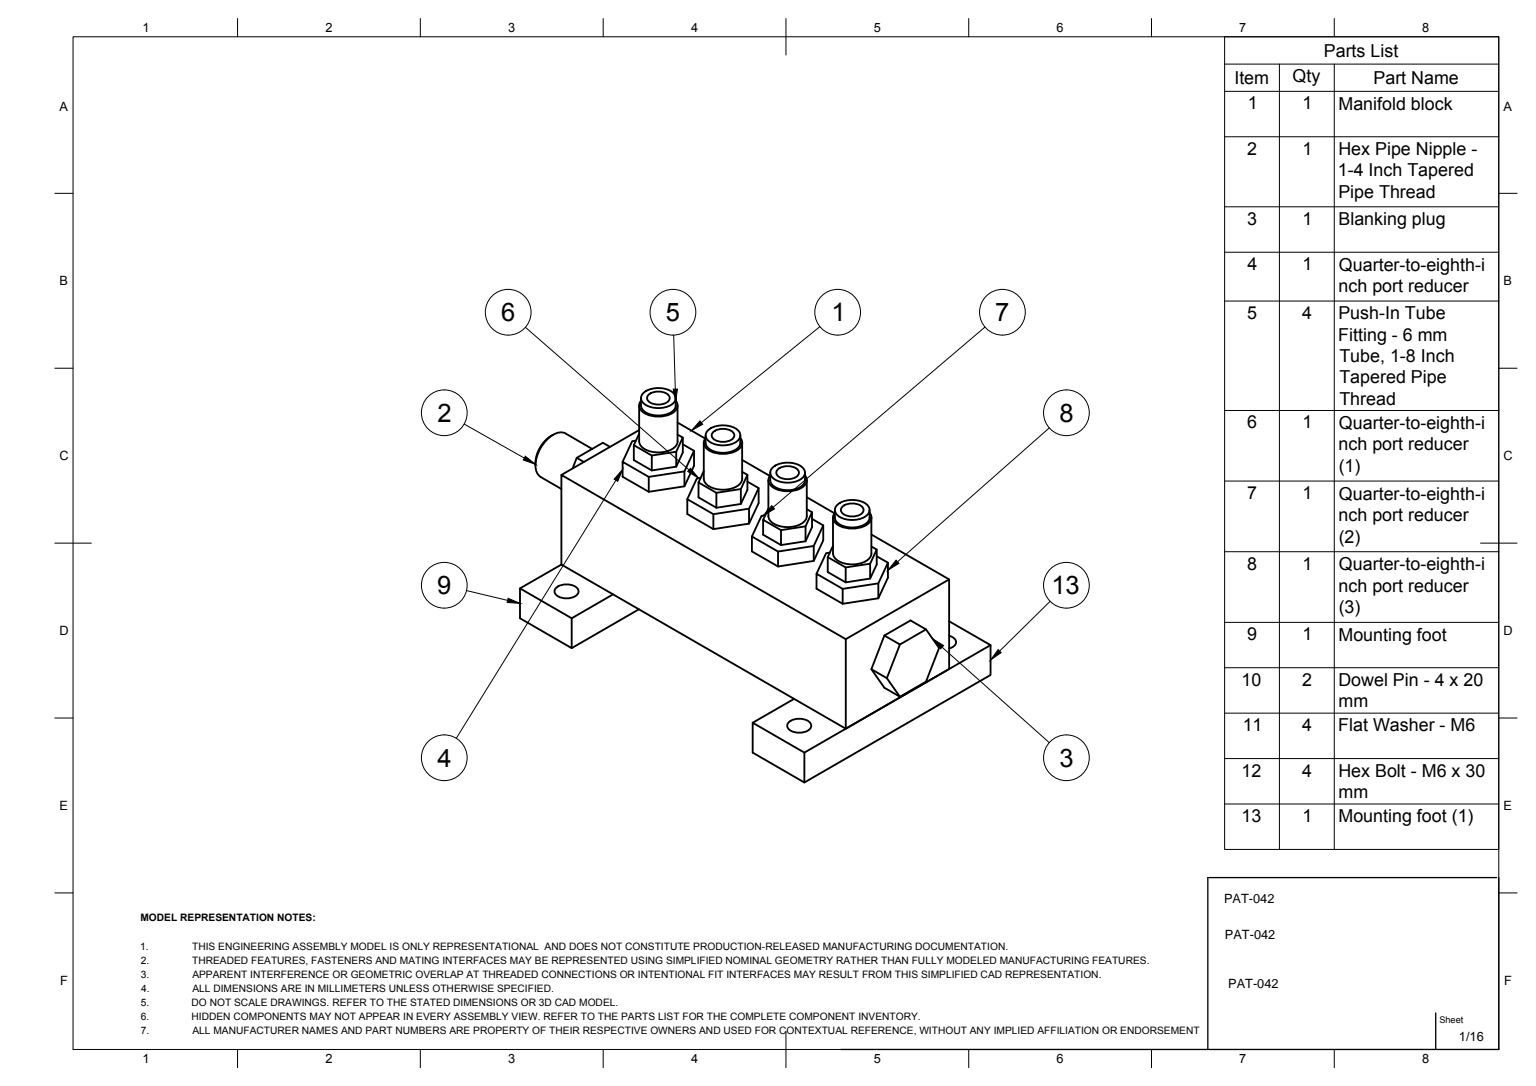
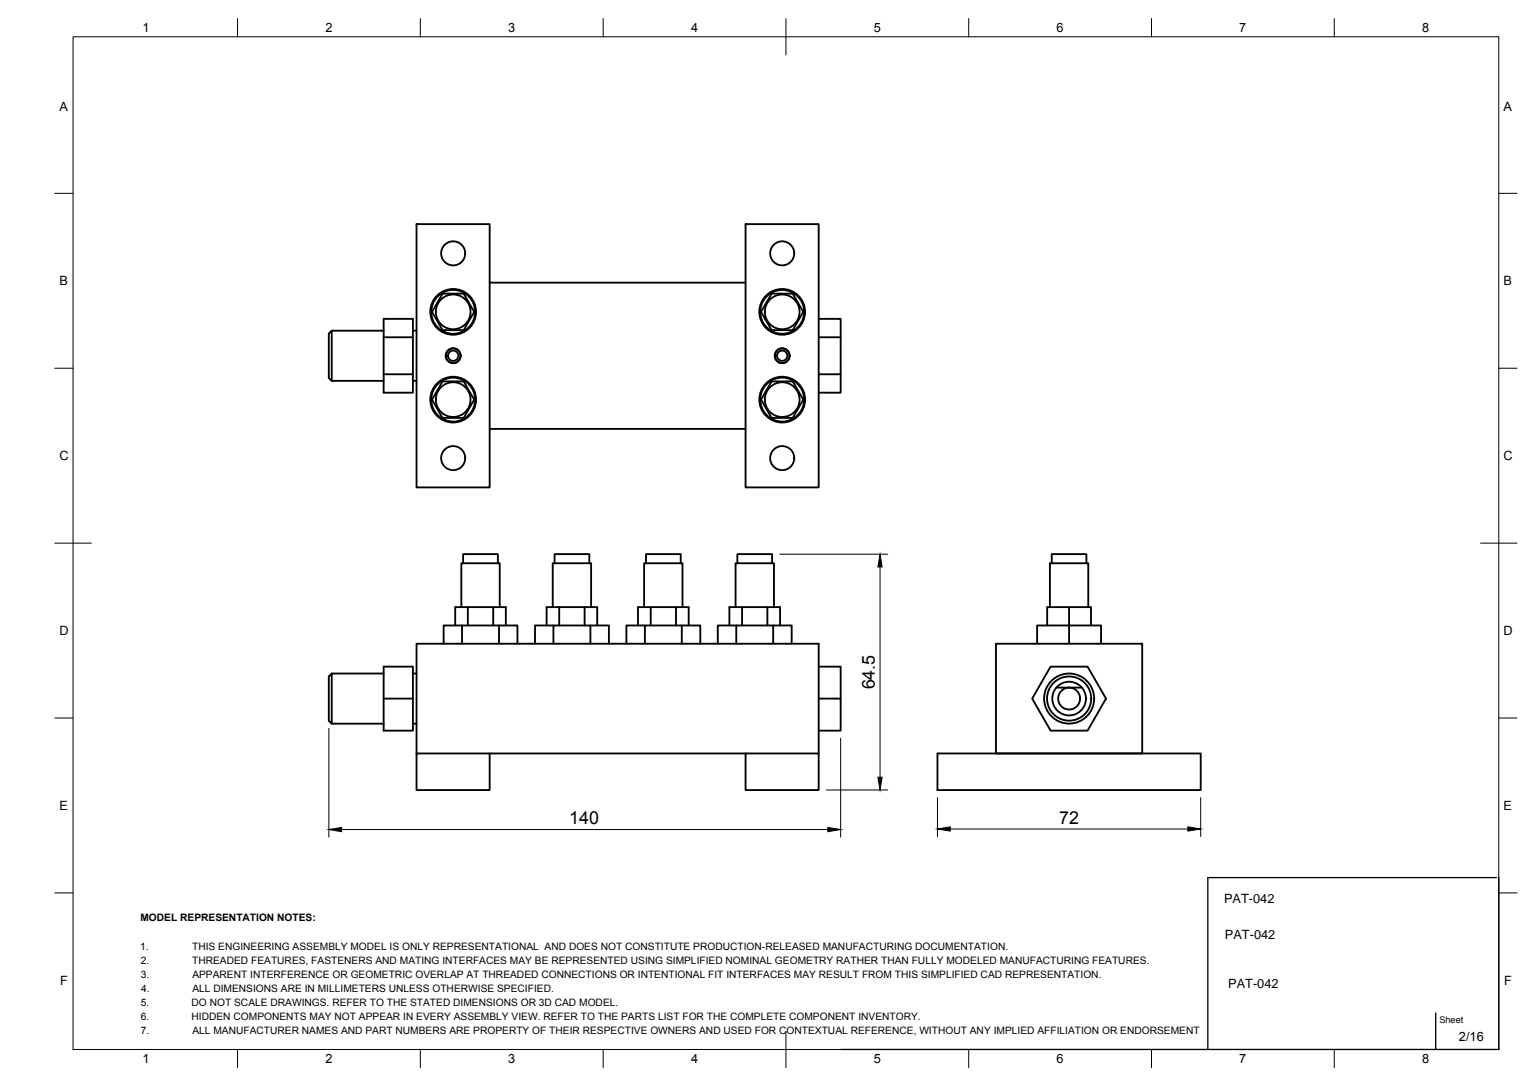
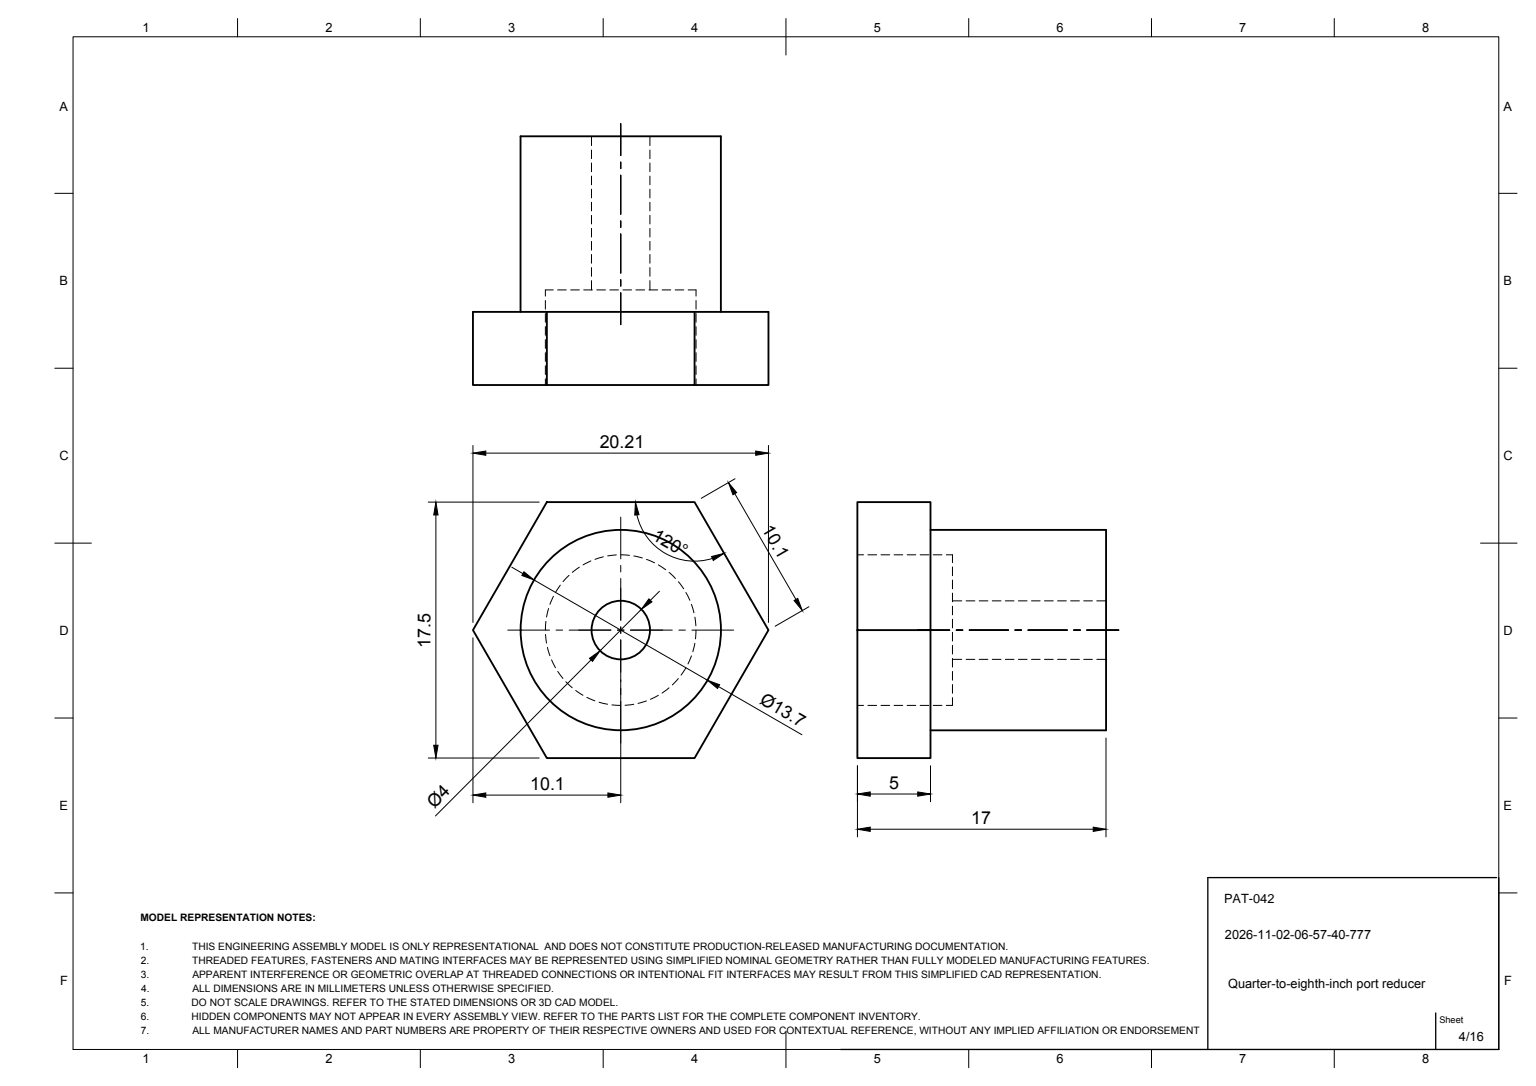
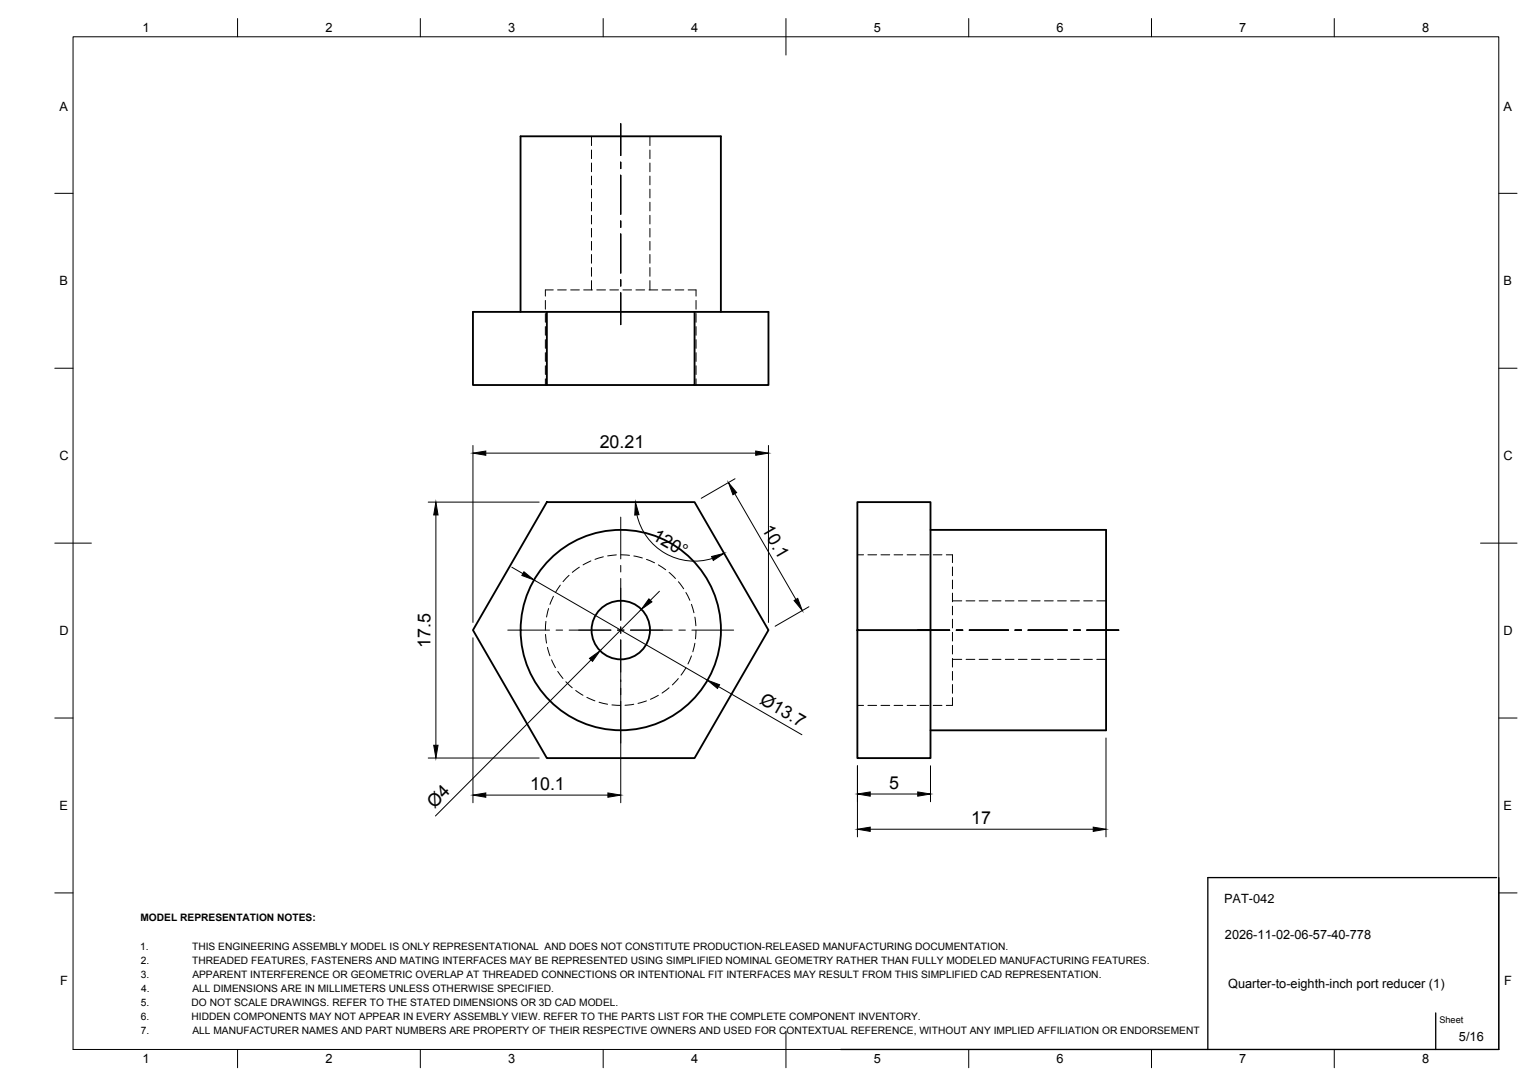
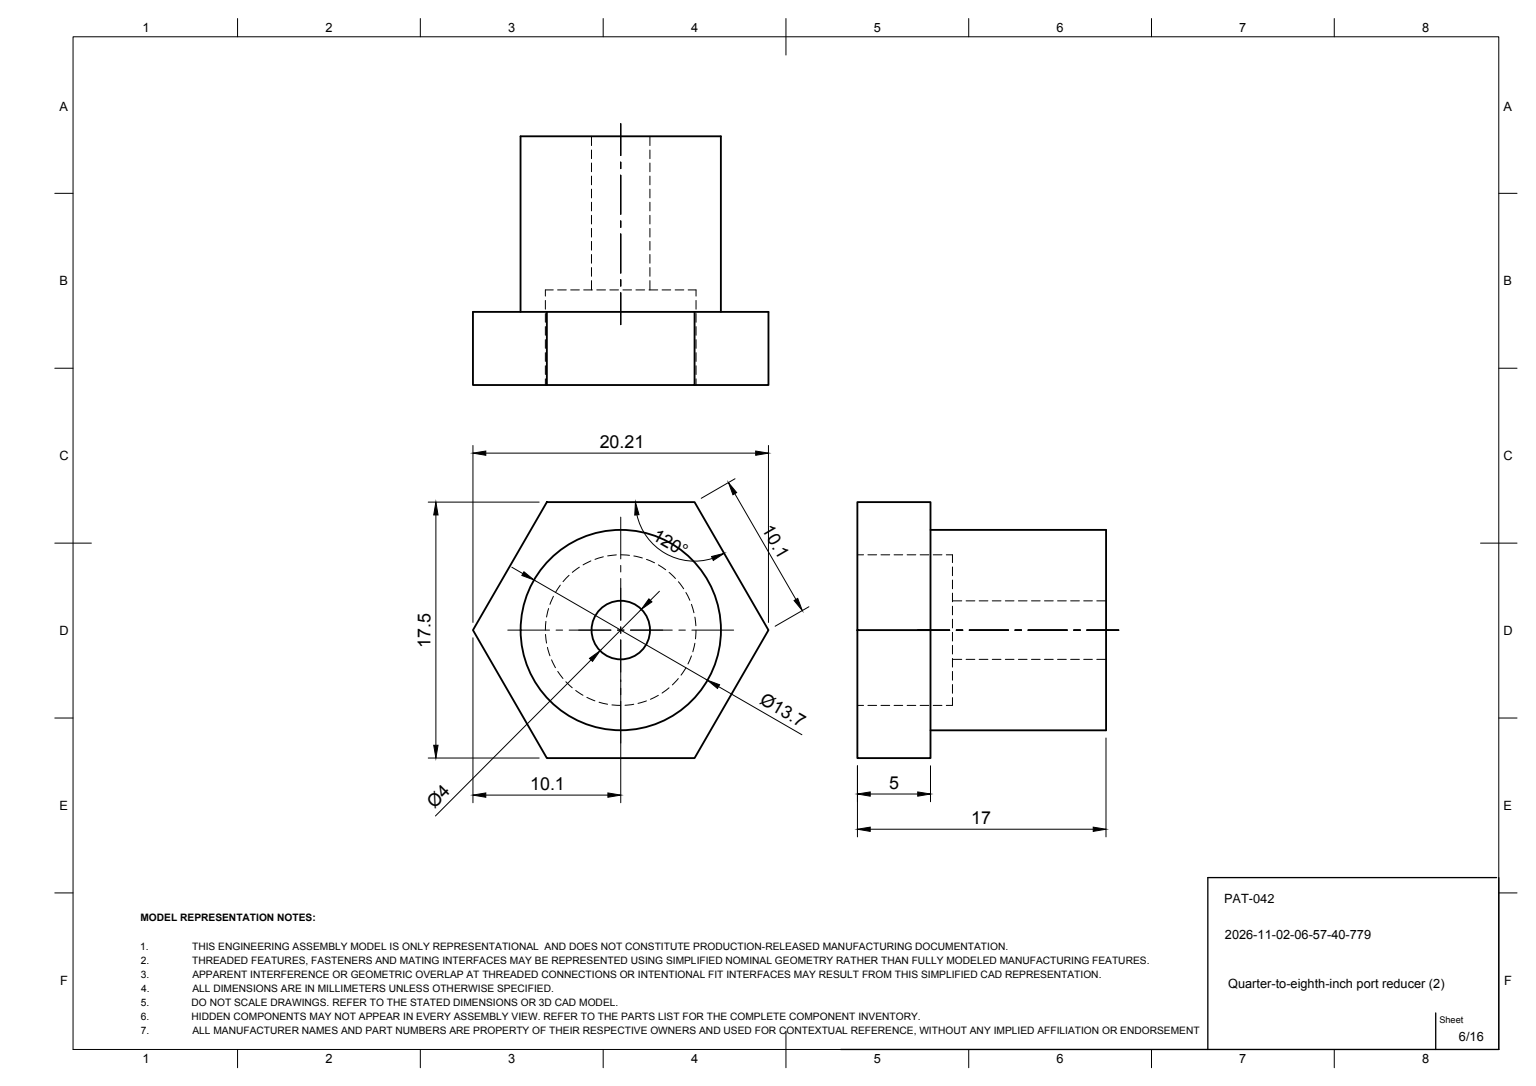
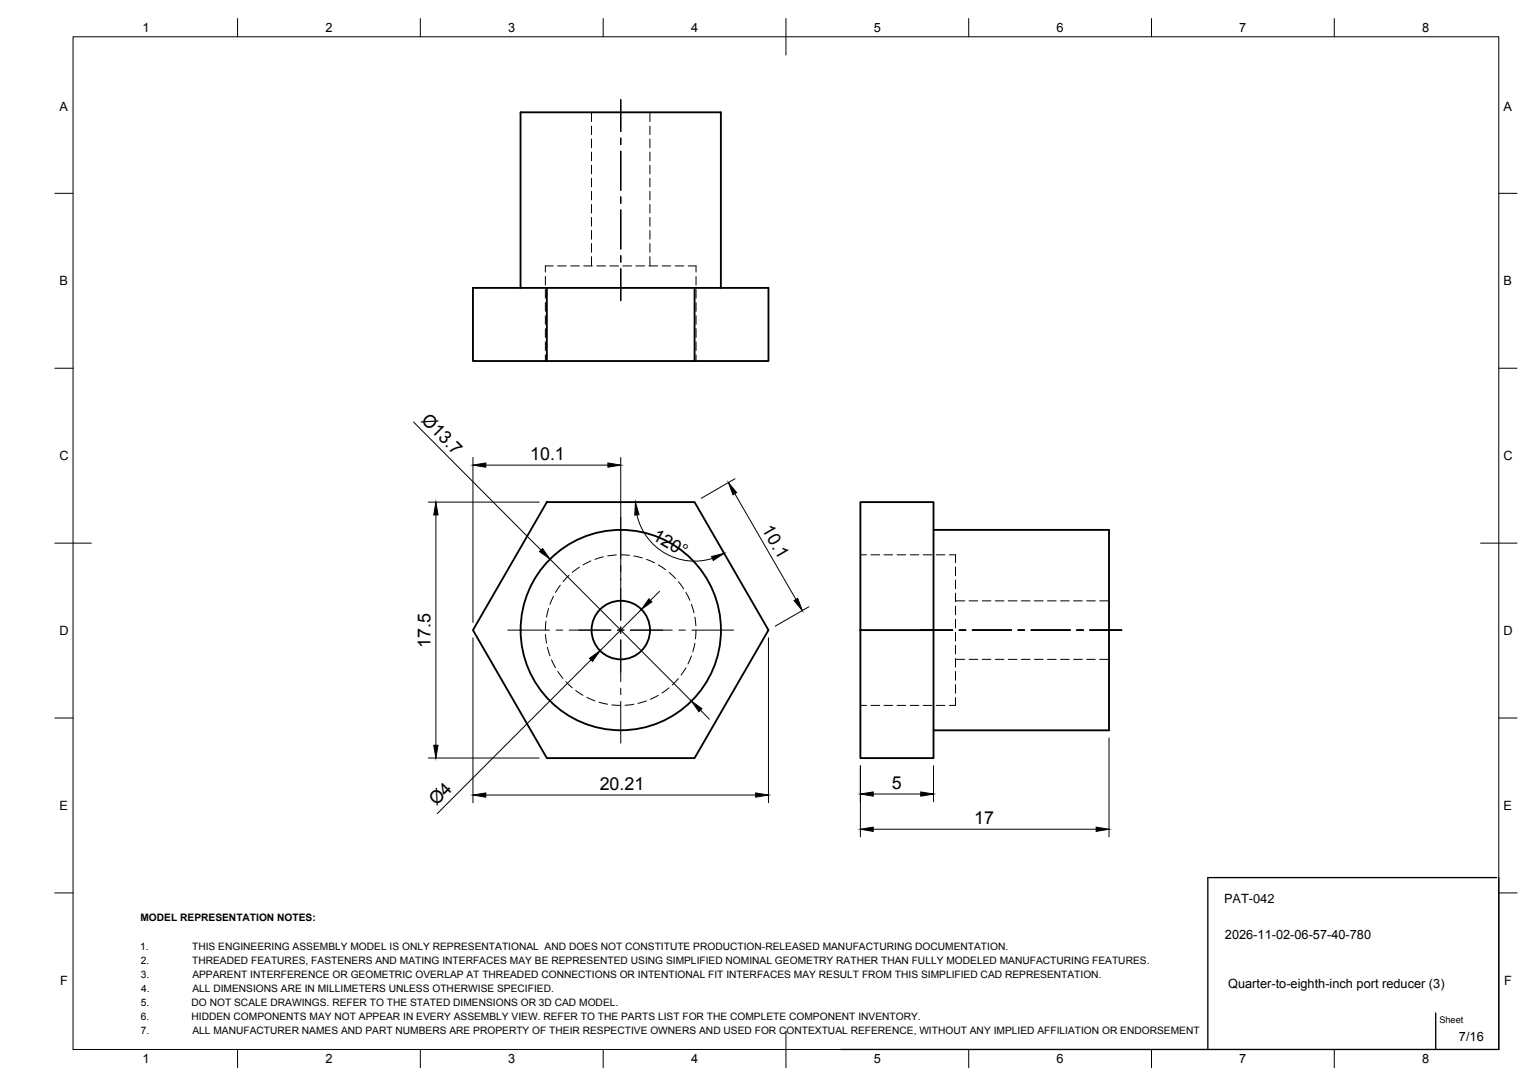
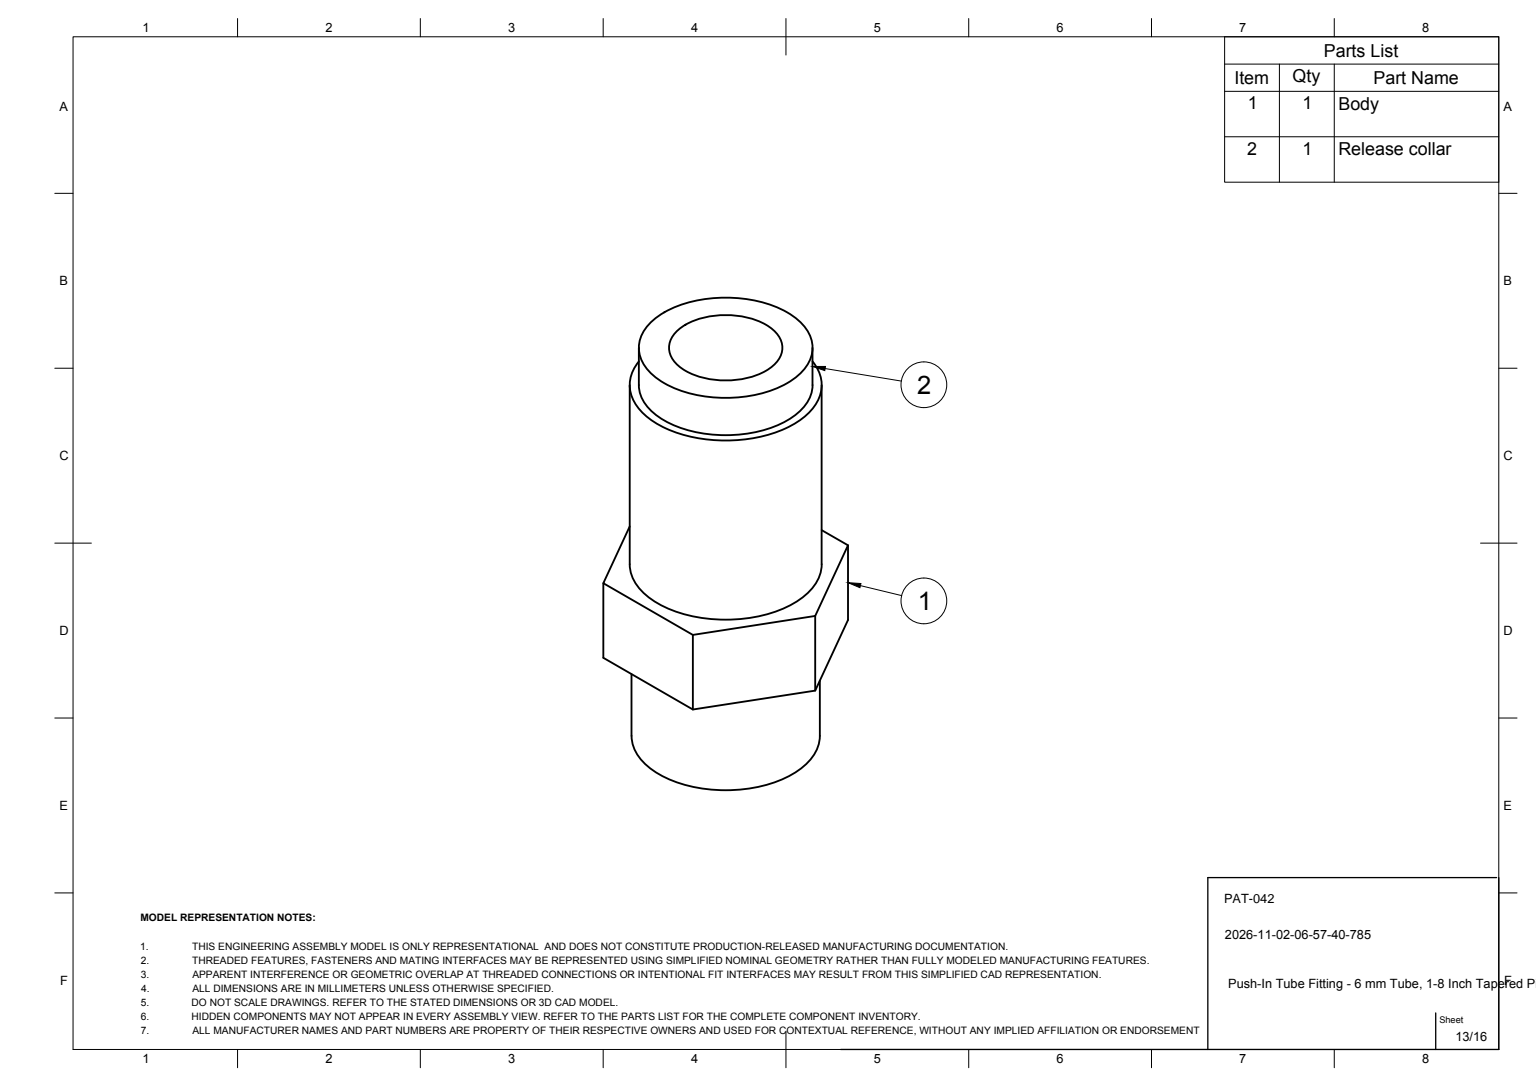
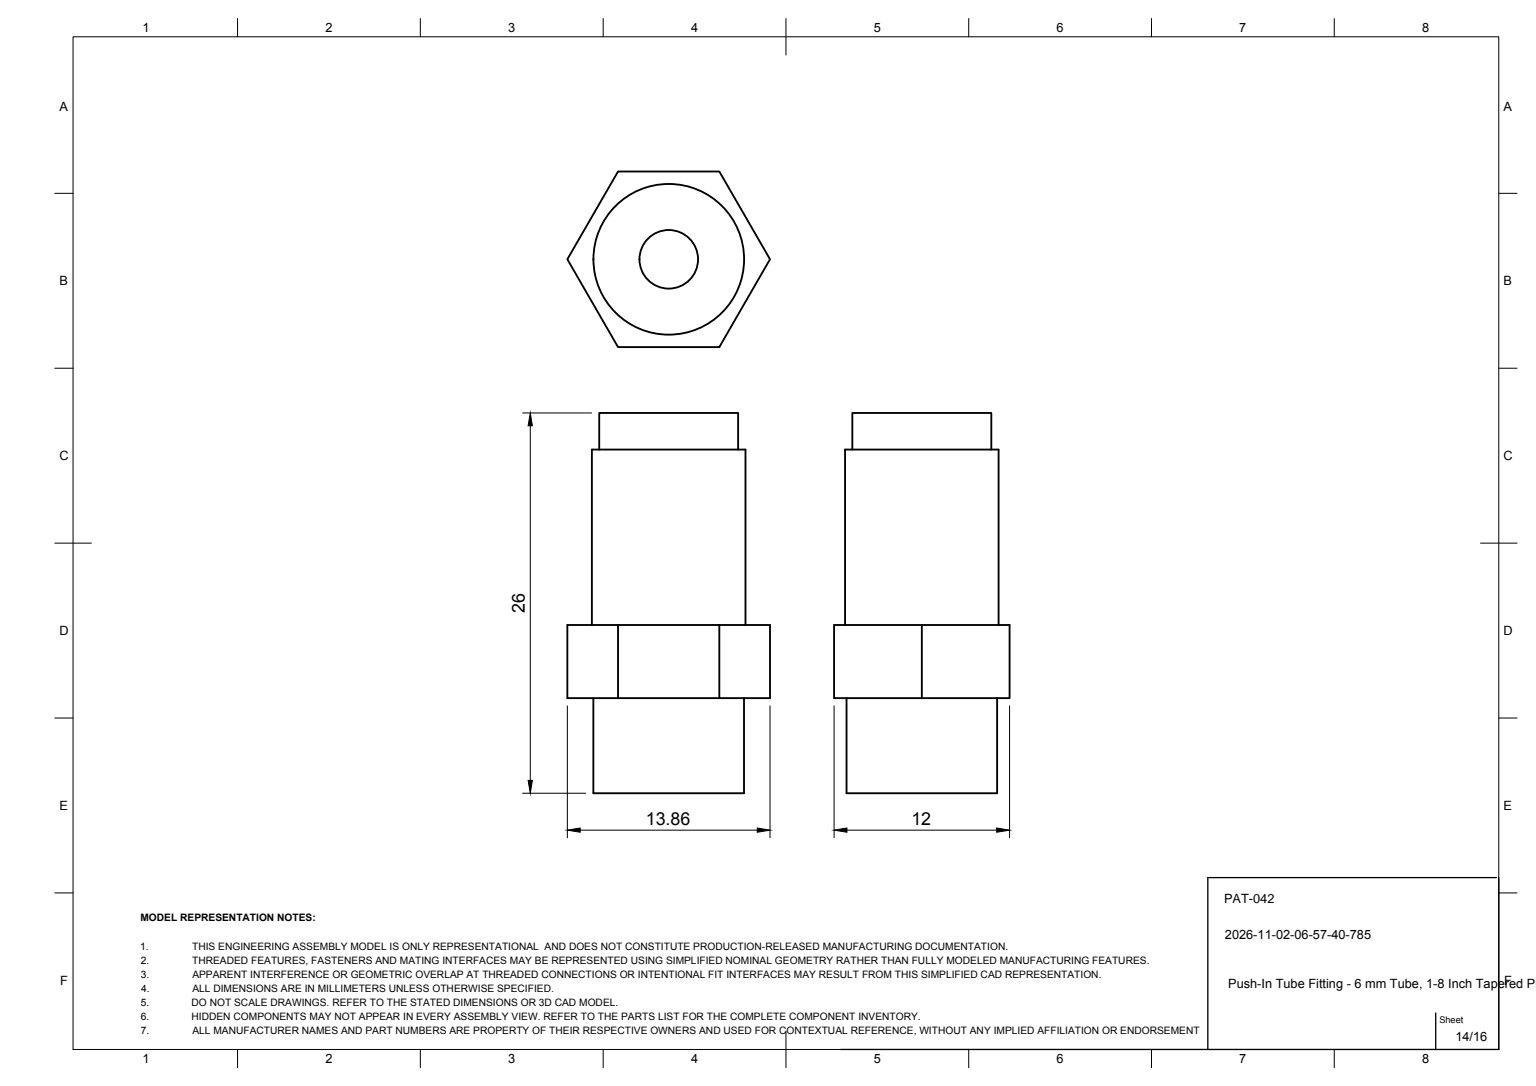
ISO-10303-21;
HEADER;
/* Generated by software containing ST-Developer
 * from STEP Tools, Inc. (www.steptools.com) 
 */

FILE_DESCRIPTION(
/* description */ ('Manifold and mounting hardware'),
/* implementation_level */ '2;1');

FILE_NAME(
/* name */ 'PAT-042',
/* time_stamp */ '2026-10-28T21:46:49-07:00',
/* author */ (''),
/* organization */ (''),
/* preprocessor_version */ 'ST-DEVELOPER v20.2',
/* originating_system */ 'Autodesk Translation Framework v15.17.0.0',
/* authorisation */ '');

FILE_SCHEMA (('AUTOMOTIVE_DESIGN { 1 0 10303 214 3 1 1 }'));
ENDSEC;

DATA;
#10=MECHANICAL_DESIGN_GEOMETRIC_PRESENTATION_REPRESENTATION('',(#150,#151,
#152,#153,#154,#155,#156,#157,#158,#159,#160,#161,#162,#163),#5638);
#11=(
BOUNDED_CURVE()
B_SPLINE_CURVE(2,(#5534,#5535,#5536),.UNSPECIFIED.,.F.,.F.)
B_SPLINE_CURVE_WITH_KNOTS((3,3),(0.144988513094728,0.791574906712449),
 .UNSPECIFIED.)
CURVE()
GEOMETRIC_REPRESENTATION_ITEM()
RATIONAL_B_SPLINE_CURVE((1.09282032302755,1.26188021535082,1.09282032302931))
REPRESENTATION_ITEM('')
);
#12=(
BOUNDED_CURVE()
B_SPLINE_CURVE(2,(#5538,#5539,#5540),.UNSPECIFIED.,.F.,.F.)
B_SPLINE_CURVE_WITH_KNOTS((3,3),(0.144988513094728,0.791574906712449),
 .UNSPECIFIED.)
CURVE()
GEOMETRIC_REPRESENTATION_ITEM()
RATIONAL_B_SPLINE_CURVE((1.09282032302755,1.26188021535082,1.09282032302931))
REPRESENTATION_ITEM('')
);
#13=(
BOUNDED_CURVE()
B_SPLINE_CURVE(2,(#5542,#5543,#5544),.UNSPECIFIED.,.F.,.F.)
B_SPLINE_CURVE_WITH_KNOTS((3,3),(0.144988513094728,0.791574906712449),
 .UNSPECIFIED.)
CURVE()
GEOMETRIC_REPRESENTATION_ITEM()
RATIONAL_B_SPLINE_CURVE((1.09282032302755,1.26188021535082,1.09282032302931))
REPRESENTATION_ITEM('')
);
#14=(
BOUNDED_CURVE()
B_SPLINE_CURVE(2,(#5546,#5547,#5548),.UNSPECIFIED.,.F.,.F.)
B_SPLINE_CURVE_WITH_KNOTS((3,3),(0.144988513094728,0.791574906712449),
 .UNSPECIFIED.)
CURVE()
GEOMETRIC_REPRESENTATION_ITEM()
RATIONAL_B_SPLINE_CURVE((1.09282032302755,1.26188021535082,1.09282032302931))
REPRESENTATION_ITEM('')
);
#15=(
BOUNDED_CURVE()
B_SPLINE_CURVE(2,(#5550,#5551,#5552),.UNSPECIFIED.,.F.,.F.)
B_SPLINE_CURVE_WITH_KNOTS((3,3),(0.144988513094728,0.791574906712449),
 .UNSPECIFIED.)
CURVE()
GEOMETRIC_REPRESENTATION_ITEM()
RATIONAL_B_SPLINE_CURVE((1.09282032302755,1.26188021535082,1.09282032302931))
REPRESENTATION_ITEM('')
);
#16=(
BOUNDED_CURVE()
B_SPLINE_CURVE(2,(#5553,#5554,#5555),.UNSPECIFIED.,.F.,.F.)
B_SPLINE_CURVE_WITH_KNOTS((3,3),(0.144988513094727,0.791574906712449),
 .UNSPECIFIED.)
CURVE()
GEOMETRIC_REPRESENTATION_ITEM()
RATIONAL_B_SPLINE_CURVE((1.09282032302755,1.26188021535082,1.09282032302931))
REPRESENTATION_ITEM('')
);
#17=SPHERICAL_SURFACE('',#3616,0.399999999999996);
#18=ITEM_DEFINED_TRANSFORMATION($,$,#3572,#3613);
#19=ITEM_DEFINED_TRANSFORMATION($,$,#3600,#3614);
#20=ITEM_DEFINED_TRANSFORMATION($,$,#3310,#3649);
#21=ITEM_DEFINED_TRANSFORMATION($,$,#3396,#3650);
#22=ITEM_DEFINED_TRANSFORMATION($,$,#3416,#3651);
#23=ITEM_DEFINED_TRANSFORMATION($,$,#3436,#3652);
#24=ITEM_DEFINED_TRANSFORMATION($,$,#3456,#3653);
#25=ITEM_DEFINED_TRANSFORMATION($,$,#3476,#3654);
#26=ITEM_DEFINED_TRANSFORMATION($,$,#3506,#3655);
#27=ITEM_DEFINED_TRANSFORMATION($,$,#3536,#3656);
#28=ITEM_DEFINED_TRANSFORMATION($,$,#3558,#3657);
#29=ITEM_DEFINED_TRANSFORMATION($,$,#3571,#3658);
#30=ITEM_DEFINED_TRANSFORMATION($,$,#3571,#3659);
#31=ITEM_DEFINED_TRANSFORMATION($,$,#3571,#3660);
#32=ITEM_DEFINED_TRANSFORMATION($,$,#3571,#3661);
#33=ITEM_DEFINED_TRANSFORMATION($,$,#3615,#3662);
#34=ITEM_DEFINED_TRANSFORMATION($,$,#3623,#3663);
#35=ITEM_DEFINED_TRANSFORMATION($,$,#3632,#3664);
#36=ITEM_DEFINED_TRANSFORMATION($,$,#3623,#3665);
#37=ITEM_DEFINED_TRANSFORMATION($,$,#3632,#3666);
#38=ITEM_DEFINED_TRANSFORMATION($,$,#3615,#3667);
#39=ITEM_DEFINED_TRANSFORMATION($,$,#3623,#3668);
#40=ITEM_DEFINED_TRANSFORMATION($,$,#3632,#3669);
#41=ITEM_DEFINED_TRANSFORMATION($,$,#3623,#3670);
#42=ITEM_DEFINED_TRANSFORMATION($,$,#3632,#3671);
#43=(
REPRESENTATION_RELATIONSHIP($,$,#5711,#5710)
REPRESENTATION_RELATIONSHIP_WITH_TRANSFORMATION(#18)
SHAPE_REPRESENTATION_RELATIONSHIP()
);
#44=(
REPRESENTATION_RELATIONSHIP($,$,#5712,#5710)
REPRESENTATION_RELATIONSHIP_WITH_TRANSFORMATION(#19)
SHAPE_REPRESENTATION_RELATIONSHIP()
);
#45=(
REPRESENTATION_RELATIONSHIP($,$,#5701,#5700)
REPRESENTATION_RELATIONSHIP_WITH_TRANSFORMATION(#20)
SHAPE_REPRESENTATION_RELATIONSHIP()
);
#46=(
REPRESENTATION_RELATIONSHIP($,$,#5702,#5700)
REPRESENTATION_RELATIONSHIP_WITH_TRANSFORMATION(#21)
SHAPE_REPRESENTATION_RELATIONSHIP()
);
#47=(
REPRESENTATION_RELATIONSHIP($,$,#5703,#5700)
REPRESENTATION_RELATIONSHIP_WITH_TRANSFORMATION(#22)
SHAPE_REPRESENTATION_RELATIONSHIP()
);
#48=(
REPRESENTATION_RELATIONSHIP($,$,#5704,#5700)
REPRESENTATION_RELATIONSHIP_WITH_TRANSFORMATION(#23)
SHAPE_REPRESENTATION_RELATIONSHIP()
);
#49=(
REPRESENTATION_RELATIONSHIP($,$,#5705,#5700)
REPRESENTATION_RELATIONSHIP_WITH_TRANSFORMATION(#24)
SHAPE_REPRESENTATION_RELATIONSHIP()
);
#50=(
REPRESENTATION_RELATIONSHIP($,$,#5706,#5700)
REPRESENTATION_RELATIONSHIP_WITH_TRANSFORMATION(#25)
SHAPE_REPRESENTATION_RELATIONSHIP()
);
#51=(
REPRESENTATION_RELATIONSHIP($,$,#5707,#5700)
REPRESENTATION_RELATIONSHIP_WITH_TRANSFORMATION(#26)
SHAPE_REPRESENTATION_RELATIONSHIP()
);
#52=(
REPRESENTATION_RELATIONSHIP($,$,#5708,#5700)
REPRESENTATION_RELATIONSHIP_WITH_TRANSFORMATION(#27)
SHAPE_REPRESENTATION_RELATIONSHIP()
);
#53=(
REPRESENTATION_RELATIONSHIP($,$,#5709,#5700)
REPRESENTATION_RELATIONSHIP_WITH_TRANSFORMATION(#28)
SHAPE_REPRESENTATION_RELATIONSHIP()
);
#54=(
REPRESENTATION_RELATIONSHIP($,$,#5710,#5700)
REPRESENTATION_RELATIONSHIP_WITH_TRANSFORMATION(#29)
SHAPE_REPRESENTATION_RELATIONSHIP()
);
#55=(
REPRESENTATION_RELATIONSHIP($,$,#5710,#5700)
REPRESENTATION_RELATIONSHIP_WITH_TRANSFORMATION(#30)
SHAPE_REPRESENTATION_RELATIONSHIP()
);
#56=(
REPRESENTATION_RELATIONSHIP($,$,#5710,#5700)
REPRESENTATION_RELATIONSHIP_WITH_TRANSFORMATION(#31)
SHAPE_REPRESENTATION_RELATIONSHIP()
);
#57=(
REPRESENTATION_RELATIONSHIP($,$,#5710,#5700)
REPRESENTATION_RELATIONSHIP_WITH_TRANSFORMATION(#32)
SHAPE_REPRESENTATION_RELATIONSHIP()
);
#58=(
REPRESENTATION_RELATIONSHIP($,$,#5713,#5700)
REPRESENTATION_RELATIONSHIP_WITH_TRANSFORMATION(#33)
SHAPE_REPRESENTATION_RELATIONSHIP()
);
#59=(
REPRESENTATION_RELATIONSHIP($,$,#5714,#5700)
REPRESENTATION_RELATIONSHIP_WITH_TRANSFORMATION(#34)
SHAPE_REPRESENTATION_RELATIONSHIP()
);
#60=(
REPRESENTATION_RELATIONSHIP($,$,#5715,#5700)
REPRESENTATION_RELATIONSHIP_WITH_TRANSFORMATION(#35)
SHAPE_REPRESENTATION_RELATIONSHIP()
);
#61=(
REPRESENTATION_RELATIONSHIP($,$,#5714,#5700)
REPRESENTATION_RELATIONSHIP_WITH_TRANSFORMATION(#36)
SHAPE_REPRESENTATION_RELATIONSHIP()
);
#62=(
REPRESENTATION_RELATIONSHIP($,$,#5715,#5700)
REPRESENTATION_RELATIONSHIP_WITH_TRANSFORMATION(#37)
SHAPE_REPRESENTATION_RELATIONSHIP()
);
#63=(
REPRESENTATION_RELATIONSHIP($,$,#5713,#5700)
REPRESENTATION_RELATIONSHIP_WITH_TRANSFORMATION(#38)
SHAPE_REPRESENTATION_RELATIONSHIP()
);
#64=(
REPRESENTATION_RELATIONSHIP($,$,#5714,#5700)
REPRESENTATION_RELATIONSHIP_WITH_TRANSFORMATION(#39)
SHAPE_REPRESENTATION_RELATIONSHIP()
);
#65=(
REPRESENTATION_RELATIONSHIP($,$,#5715,#5700)
REPRESENTATION_RELATIONSHIP_WITH_TRANSFORMATION(#40)
SHAPE_REPRESENTATION_RELATIONSHIP()
);
#66=(
REPRESENTATION_RELATIONSHIP($,$,#5714,#5700)
REPRESENTATION_RELATIONSHIP_WITH_TRANSFORMATION(#41)
SHAPE_REPRESENTATION_RELATIONSHIP()
);
#67=(
REPRESENTATION_RELATIONSHIP($,$,#5715,#5700)
REPRESENTATION_RELATIONSHIP_WITH_TRANSFORMATION(#42)
SHAPE_REPRESENTATION_RELATIONSHIP()
);
#68=CONTEXT_DEPENDENT_SHAPE_REPRESENTATION(#43,#5672);
#69=CONTEXT_DEPENDENT_SHAPE_REPRESENTATION(#44,#5673);
#70=CONTEXT_DEPENDENT_SHAPE_REPRESENTATION(#45,#5677);
#71=CONTEXT_DEPENDENT_SHAPE_REPRESENTATION(#46,#5678);
#72=CONTEXT_DEPENDENT_SHAPE_REPRESENTATION(#47,#5679);
#73=CONTEXT_DEPENDENT_SHAPE_REPRESENTATION(#48,#5680);
#74=CONTEXT_DEPENDENT_SHAPE_REPRESENTATION(#49,#5681);
#75=CONTEXT_DEPENDENT_SHAPE_REPRESENTATION(#50,#5682);
#76=CONTEXT_DEPENDENT_SHAPE_REPRESENTATION(#51,#5683);
#77=CONTEXT_DEPENDENT_SHAPE_REPRESENTATION(#52,#5684);
#78=CONTEXT_DEPENDENT_SHAPE_REPRESENTATION(#53,#5685);
#79=CONTEXT_DEPENDENT_SHAPE_REPRESENTATION(#54,#5686);
#80=CONTEXT_DEPENDENT_SHAPE_REPRESENTATION(#55,#5687);
#81=CONTEXT_DEPENDENT_SHAPE_REPRESENTATION(#56,#5688);
#82=CONTEXT_DEPENDENT_SHAPE_REPRESENTATION(#57,#5689);
#83=CONTEXT_DEPENDENT_SHAPE_REPRESENTATION(#58,#5690);
#84=CONTEXT_DEPENDENT_SHAPE_REPRESENTATION(#59,#5691);
#85=CONTEXT_DEPENDENT_SHAPE_REPRESENTATION(#60,#5692);
#86=CONTEXT_DEPENDENT_SHAPE_REPRESENTATION(#61,#5693);
#87=CONTEXT_DEPENDENT_SHAPE_REPRESENTATION(#62,#5694);
#88=CONTEXT_DEPENDENT_SHAPE_REPRESENTATION(#63,#5695);
#89=CONTEXT_DEPENDENT_SHAPE_REPRESENTATION(#64,#5696);
#90=CONTEXT_DEPENDENT_SHAPE_REPRESENTATION(#65,#5697);
#91=CONTEXT_DEPENDENT_SHAPE_REPRESENTATION(#66,#5698);
#92=CONTEXT_DEPENDENT_SHAPE_REPRESENTATION(#67,#5699);
#93=NEXT_ASSEMBLY_USAGE_OCCURRENCE('Body:1','Body:1','Body:1',#5727,#5728,
'Body:1');
#94=NEXT_ASSEMBLY_USAGE_OCCURRENCE('Release collar:1',
'Release collar:1','Release collar:1',#5727,#5729,'Release collar:1');
#95=NEXT_ASSEMBLY_USAGE_OCCURRENCE('Manifold block:1',
'Manifold block:1','Manifold block:1',#5717,#5718,'Manifold block:1');
#96=NEXT_ASSEMBLY_USAGE_OCCURRENCE('1/4-1/8 in port reducer (3):1',
'1/4-1/8 in port reducer (3):1','1/4-1/8 in port reducer (3):1',#5717,#5719,
'1/4-1/8 in port reducer (3):1');
#97=NEXT_ASSEMBLY_USAGE_OCCURRENCE('1/4-1/8 in port reducer:1',
'1/4-1/8 in port reducer:1','1/4-1/8 in port reducer:1',#5717,#5720,
'1/4-1/8 in port reducer:1');
#98=NEXT_ASSEMBLY_USAGE_OCCURRENCE('1/4-1/8 in port reducer (1):1',
'1/4-1/8 in port reducer (1):1','1/4-1/8 in port reducer (1):1',#5717,#5721,
'1/4-1/8 in port reducer (1):1');
#99=NEXT_ASSEMBLY_USAGE_OCCURRENCE('1/4-1/8 in port reducer (2):1',
'1/4-1/8 in port reducer (2):1','1/4-1/8 in port reducer (2):1',#5717,#5722,
'1/4-1/8 in port reducer (2):1');
#100=NEXT_ASSEMBLY_USAGE_OCCURRENCE('Mounting foot:1','Mounting foot:1',
'Mounting foot:1',#5717,#5723,'Mounting foot:1');
#101=NEXT_ASSEMBLY_USAGE_OCCURRENCE('Mounting foot (1):1',
'Mounting foot (1):1','Mounting foot (1):1',#5717,#5724,
'Mounting foot (1):1');
#102=NEXT_ASSEMBLY_USAGE_OCCURRENCE(
'Hex Pipe Nipple - 1-4 Inch Tapered Pipe Thread:1',
'Hex Pipe Nipple - 1-4 Inch Tapered Pipe Thread:1',
'Hex Pipe Nipple - 1-4 Inch Tapered Pipe Thread:1',#5717,#5725,
'Hex Pipe Nipple - 1-4 Inch Tapered Pipe Thread:1');
#103=NEXT_ASSEMBLY_USAGE_OCCURRENCE('Blanking plug:1','Blanking plug:1',
'Blanking plug:1',#5717,#5726,'Blanking plug:1');
#104=NEXT_ASSEMBLY_USAGE_OCCURRENCE(
'Push-In Tube Fitting - 6 mm Tube, 1-8 Inch Tapered Pipe Thread:1',
'Push-In Tube Fitting - 6 mm Tube, 1-8 Inch Tapered Pipe Thread:1',
'Push-In Tube Fitting - 6 mm Tube, 1-8 Inch Tapered Pipe Thread:1',#5717,
#5727,
'Push-In Tube Fitting - 6 mm Tube, 1-8 Inch Tapered Pipe Thread:1');
#105=NEXT_ASSEMBLY_USAGE_OCCURRENCE(
'Push-In Tube Fitting - 6 mm Tube, 1-8 Inch Tapered Pipe Thread:2',
'Push-In Tube Fitting - 6 mm Tube, 1-8 Inch Tapered Pipe Thread:2',
'Push-In Tube Fitting - 6 mm Tube, 1-8 Inch Tapered Pipe Thread:2',#5717,
#5727,
'Push-In Tube Fitting - 6 mm Tube, 1-8 Inch Tapered Pipe Thread:2');
#106=NEXT_ASSEMBLY_USAGE_OCCURRENCE(
'Push-In Tube Fitting - 6 mm Tube, 1-8 Inch Tapered Pipe Thread:3',
'Push-In Tube Fitting - 6 mm Tube, 1-8 Inch Tapered Pipe Thread:3',
'Push-In Tube Fitting - 6 mm Tube, 1-8 Inch Tapered Pipe Thread:3',#5717,
#5727,
'Push-In Tube Fitting - 6 mm Tube, 1-8 Inch Tapered Pipe Thread:3');
#107=NEXT_ASSEMBLY_USAGE_OCCURRENCE(
'Push-In Tube Fitting - 6 mm Tube, 1-8 Inch Tapered Pipe Thread:4',
'Push-In Tube Fitting - 6 mm Tube, 1-8 Inch Tapered Pipe Thread:4',
'Push-In Tube Fitting - 6 mm Tube, 1-8 Inch Tapered Pipe Thread:4',#5717,
#5727,
'Push-In Tube Fitting - 6 mm Tube, 1-8 Inch Tapered Pipe Thread:4');
#108=NEXT_ASSEMBLY_USAGE_OCCURRENCE('Dowel Pin - 4 x 20 mm:1',
'Dowel Pin - 4 x 20 mm:1','Dowel Pin - 4 x 20 mm:1',#5717,#5730,
'Dowel Pin - 4 x 20 mm:1');
#109=NEXT_ASSEMBLY_USAGE_OCCURRENCE('Flat Washer - M6:1',
'Flat Washer - M6:1','Flat Washer - M6:1',#5717,#5731,
'Flat Washer - M6:1');
#110=NEXT_ASSEMBLY_USAGE_OCCURRENCE('Hex Bolt - M6 x 30 mm:1',
'Hex Bolt - M6 x 30 mm:1','Hex Bolt - M6 x 30 mm:1',#5717,#5732,
'Hex Bolt - M6 x 30 mm:1');
#111=NEXT_ASSEMBLY_USAGE_OCCURRENCE('Flat Washer - M6:2',
'Flat Washer - M6:2','Flat Washer - M6:2',#5717,#5731,
'Flat Washer - M6:2');
#112=NEXT_ASSEMBLY_USAGE_OCCURRENCE('Hex Bolt - M6 x 30 mm:2',
'Hex Bolt - M6 x 30 mm:2','Hex Bolt - M6 x 30 mm:2',#5717,#5732,
'Hex Bolt - M6 x 30 mm:2');
#113=NEXT_ASSEMBLY_USAGE_OCCURRENCE('Dowel Pin - 4 x 20 mm:2',
'Dowel Pin - 4 x 20 mm:2','Dowel Pin - 4 x 20 mm:2',#5717,#5730,
'Dowel Pin - 4 x 20 mm:2');
#114=NEXT_ASSEMBLY_USAGE_OCCURRENCE('Flat Washer - M6:3',
'Flat Washer - M6:3','Flat Washer - M6:3',#5717,#5731,
'Flat Washer - M6:3');
#115=NEXT_ASSEMBLY_USAGE_OCCURRENCE('Hex Bolt - M6 x 30 mm:3',
'Hex Bolt - M6 x 30 mm:3','Hex Bolt - M6 x 30 mm:3',#5717,#5732,
'Hex Bolt - M6 x 30 mm:3');
#116=NEXT_ASSEMBLY_USAGE_OCCURRENCE('Flat Washer - M6:4',
'Flat Washer - M6:4','Flat Washer - M6:4',#5717,#5731,
'Flat Washer - M6:4');
#117=NEXT_ASSEMBLY_USAGE_OCCURRENCE('Hex Bolt - M6 x 30 mm:4',
'Hex Bolt - M6 x 30 mm:4','Hex Bolt - M6 x 30 mm:4',#5717,#5732,
'Hex Bolt - M6 x 30 mm:4');
#118=CONICAL_SURFACE('',#3555,0.645,0.785398163397448);
#119=CONICAL_SURFACE('',#3620,0.17,0.785398163397449);
#120=CONICAL_SURFACE('',#3636,0.27,0.785398163397448);
#121=CONICAL_SURFACE('',#3639,0.576175134594813,1.0471975511966);
#122=SHAPE_REPRESENTATION_RELATIONSHIP('SRR','None',#5701,#136);
#123=SHAPE_REPRESENTATION_RELATIONSHIP('SRR','None',#5702,#137);
#124=SHAPE_REPRESENTATION_RELATIONSHIP('SRR','None',#5703,#138);
#125=SHAPE_REPRESENTATION_RELATIONSHIP('SRR','None',#5704,#139);
#126=SHAPE_REPRESENTATION_RELATIONSHIP('SRR','None',#5705,#140);
#127=SHAPE_REPRESENTATION_RELATIONSHIP('SRR','None',#5706,#141);
#128=SHAPE_REPRESENTATION_RELATIONSHIP('SRR','None',#5707,#142);
#129=SHAPE_REPRESENTATION_RELATIONSHIP('SRR','None',#5708,#143);
#130=SHAPE_REPRESENTATION_RELATIONSHIP('SRR','None',#5709,#144);
#131=SHAPE_REPRESENTATION_RELATIONSHIP('SRR','None',#5711,#145);
#132=SHAPE_REPRESENTATION_RELATIONSHIP('SRR','None',#5712,#146);
#133=SHAPE_REPRESENTATION_RELATIONSHIP('SRR','None',#5713,#147);
#134=SHAPE_REPRESENTATION_RELATIONSHIP('SRR','None',#5714,#148);
#135=SHAPE_REPRESENTATION_RELATIONSHIP('SRR','None',#5715,#149);
#136=ADVANCED_BREP_SHAPE_REPRESENTATION('',(#164),#5623);
#137=ADVANCED_BREP_SHAPE_REPRESENTATION('',(#165),#5624);
#138=ADVANCED_BREP_SHAPE_REPRESENTATION('',(#166),#5625);
#139=ADVANCED_BREP_SHAPE_REPRESENTATION('',(#167),#5626);
#140=ADVANCED_BREP_SHAPE_REPRESENTATION('',(#168),#5627);
#141=ADVANCED_BREP_SHAPE_REPRESENTATION('',(#169),#5628);
#142=ADVANCED_BREP_SHAPE_REPRESENTATION('',(#170),#5629);
#143=ADVANCED_BREP_SHAPE_REPRESENTATION('',(#171),#5630);
#144=ADVANCED_BREP_SHAPE_REPRESENTATION('',(#172),#5631);
#145=ADVANCED_BREP_SHAPE_REPRESENTATION('',(#173),#5633);
#146=ADVANCED_BREP_SHAPE_REPRESENTATION('',(#174),#5634);
#147=ADVANCED_BREP_SHAPE_REPRESENTATION('',(#175),#5635);
#148=ADVANCED_BREP_SHAPE_REPRESENTATION('',(#176),#5636);
#149=ADVANCED_BREP_SHAPE_REPRESENTATION('',(#177),#5637);
#150=STYLED_ITEM('',(#5839),#164);
#151=STYLED_ITEM('',(#5853),#165);
#152=STYLED_ITEM('',(#5853),#166);
#153=STYLED_ITEM('',(#5853),#167);
#154=STYLED_ITEM('',(#5853),#168);
#155=STYLED_ITEM('',(#5853),#169);
#156=STYLED_ITEM('',(#5853),#170);
#157=STYLED_ITEM('',(#5853),#171);
#158=STYLED_ITEM('',(#5874),#172);
#159=STYLED_ITEM('',(#5839),#173);
#160=STYLED_ITEM('',(#5874),#174);
#161=STYLED_ITEM('',(#5860),#175);
#162=STYLED_ITEM('',(#5867),#176);
#163=STYLED_ITEM('',(#5867),#177);
#164=MANIFOLD_SOLID_BREP('Body1',#3140);
#165=MANIFOLD_SOLID_BREP('Body1',#3141);
#166=MANIFOLD_SOLID_BREP('Body1',#3142);
#167=MANIFOLD_SOLID_BREP('Body1',#3143);
#168=MANIFOLD_SOLID_BREP('Body1',#3144);
#169=MANIFOLD_SOLID_BREP('Body1',#3145);
#170=MANIFOLD_SOLID_BREP('Body1',#3146);
#171=MANIFOLD_SOLID_BREP('Body1',#3147);
#172=MANIFOLD_SOLID_BREP('Body1',#3148);
#173=MANIFOLD_SOLID_BREP('Body1',#3149);
#174=MANIFOLD_SOLID_BREP('Body1',#3150);
#175=MANIFOLD_SOLID_BREP('Body1',#3151);
#176=MANIFOLD_SOLID_BREP('Body1',#3152);
#177=MANIFOLD_SOLID_BREP('Body1',#3153);
#178=FACE_BOUND('',#528,.T.);
#179=FACE_BOUND('',#531,.T.);
#180=FACE_BOUND('',#539,.T.);
#181=FACE_BOUND('',#542,.T.);
#182=FACE_BOUND('',#545,.T.);
#183=FACE_BOUND('',#546,.T.);
#184=FACE_BOUND('',#555,.T.);
#185=FACE_BOUND('',#558,.T.);
#186=FACE_BOUND('',#560,.T.);
#187=FACE_BOUND('',#561,.T.);
#188=FACE_BOUND('',#562,.T.);
#189=FACE_BOUND('',#563,.T.);
#190=FACE_BOUND('',#565,.T.);
#191=FACE_BOUND('',#566,.T.);
#192=FACE_BOUND('',#567,.T.);
#193=FACE_BOUND('',#568,.T.);
#194=FACE_BOUND('',#569,.T.);
#195=FACE_BOUND('',#570,.T.);
#196=FACE_BOUND('',#573,.T.);
#197=FACE_BOUND('',#575,.T.);
#198=FACE_BOUND('',#583,.T.);
#199=FACE_BOUND('',#587,.T.);
#200=FACE_BOUND('',#590,.T.);
#201=FACE_BOUND('',#592,.T.);
#202=FACE_BOUND('',#600,.T.);
#203=FACE_BOUND('',#604,.T.);
#204=FACE_BOUND('',#607,.T.);
#205=FACE_BOUND('',#609,.T.);
#206=FACE_BOUND('',#617,.T.);
#207=FACE_BOUND('',#621,.T.);
#208=FACE_BOUND('',#624,.T.);
#209=FACE_BOUND('',#626,.T.);
#210=FACE_BOUND('',#634,.T.);
#211=FACE_BOUND('',#638,.T.);
#212=FACE_BOUND('',#644,.T.);
#213=FACE_BOUND('',#647,.T.);
#214=FACE_BOUND('',#655,.T.);
#215=FACE_BOUND('',#656,.T.);
#216=FACE_BOUND('',#657,.T.);
#217=FACE_BOUND('',#658,.T.);
#218=FACE_BOUND('',#659,.T.);
#219=FACE_BOUND('',#661,.T.);
#220=FACE_BOUND('',#662,.T.);
#221=FACE_BOUND('',#663,.T.);
#222=FACE_BOUND('',#664,.T.);
#223=FACE_BOUND('',#665,.T.);
#224=FACE_BOUND('',#671,.T.);
#225=FACE_BOUND('',#674,.T.);
#226=FACE_BOUND('',#682,.T.);
#227=FACE_BOUND('',#683,.T.);
#228=FACE_BOUND('',#684,.T.);
#229=FACE_BOUND('',#685,.T.);
#230=FACE_BOUND('',#686,.T.);
#231=FACE_BOUND('',#688,.T.);
#232=FACE_BOUND('',#689,.T.);
#233=FACE_BOUND('',#690,.T.);
#234=FACE_BOUND('',#691,.T.);
#235=FACE_BOUND('',#692,.T.);
#236=FACE_BOUND('',#694,.T.);
#237=FACE_BOUND('',#697,.T.);
#238=FACE_BOUND('',#699,.T.);
#239=FACE_BOUND('',#710,.T.);
#240=FACE_BOUND('',#714,.T.);
#241=FACE_BOUND('',#724,.T.);
#242=FACE_BOUND('',#726,.T.);
#243=FACE_BOUND('',#728,.T.);
#244=FACE_BOUND('',#736,.T.);
#245=FACE_BOUND('',#739,.T.);
#246=FACE_BOUND('',#743,.T.);
#247=FACE_BOUND('',#746,.T.);
#248=FACE_BOUND('',#749,.T.);
#249=FACE_BOUND('',#752,.T.);
#250=FACE_BOUND('',#761,.T.);
#251=FACE_BOUND('',#763,.T.);
#252=FACE_BOUND('',#776,.T.);
#253=B_SPLINE_CURVE_WITH_KNOTS('',3,(#4697,#4698,#4699,#4700,#4701,#4702,
#4703,#4704,#4705,#4706),.UNSPECIFIED.,.F.,.F.,(4,2,2,2,4),(0.,0.0777490769060827,
0.155498153812165,0.233224303462309,0.310950453112452),.UNSPECIFIED.);
#254=B_SPLINE_CURVE_WITH_KNOTS('',3,(#4707,#4708,#4709,#4710,#4711,#4712,
#4713,#4714,#4715,#4716,#4717,#4718,#4719,#4720,#4721,#4722,#4723,#4724,
#4725,#4726,#4727,#4728,#4729,#4730,#4731,#4732),.UNSPECIFIED.,.F.,.F.,
(4,2,2,2,2,2,2,2,2,2,2,2,4),(0.310950453112452,0.388676602762596,0.466402752412739,
0.544151829318822,0.621900906224905,0.699649983130987,0.77739906003707,
0.855125209687213,0.932851359337357,1.0105775089875,1.08830365863764,1.16605273554373,
1.24380181244981),.UNSPECIFIED.);
#255=B_SPLINE_CURVE_WITH_KNOTS('',3,(#4767,#4768,#4769,#4770,#4771,#4772,
#4773,#4774,#4775,#4776),.UNSPECIFIED.,.F.,.F.,(4,2,2,2,4),(0.,0.0777490769060827,
0.155498153812165,0.233224303462309,0.310950453112452),.UNSPECIFIED.);
#256=B_SPLINE_CURVE_WITH_KNOTS('',3,(#4777,#4778,#4779,#4780,#4781,#4782,
#4783,#4784,#4785,#4786,#4787,#4788,#4789,#4790,#4791,#4792,#4793,#4794,
#4795,#4796,#4797,#4798,#4799,#4800,#4801,#4802),.UNSPECIFIED.,.F.,.F.,
(4,2,2,2,2,2,2,2,2,2,2,2,4),(0.310950453112452,0.388676602762596,0.466402752412739,
0.544151829318822,0.621900906224905,0.699649983130987,0.77739906003707,
0.855125209687213,0.932851359337357,1.0105775089875,1.08830365863764,1.16605273554373,
1.24380181244981),.UNSPECIFIED.);
#257=ELLIPSE('',#3314,0.96873629022557,0.685);
#258=ELLIPSE('',#3315,0.96873629022557,0.685);
#259=ELLIPSE('',#3316,0.96873629022557,0.685);
#260=ELLIPSE('',#3318,0.96873629022557,0.685);
#261=ELLIPSE('',#3325,0.96873629022557,0.685);
#262=ELLIPSE('',#3327,0.96873629022557,0.685);
#263=ELLIPSE('',#3329,0.96873629022557,0.685);
#264=ELLIPSE('',#3330,0.96873629022557,0.685);
#265=ELLIPSE('',#3371,0.96873629022557,0.685);
#266=ELLIPSE('',#3372,0.96873629022557,0.685);
#267=ELLIPSE('',#3373,0.96873629022557,0.685);
#268=ELLIPSE('',#3374,0.96873629022557,0.685);
#269=ELLIPSE('',#3376,0.96873629022557,0.685);
#270=ELLIPSE('',#3377,0.96873629022557,0.685);
#271=ELLIPSE('',#3378,0.96873629022557,0.685);
#272=ELLIPSE('',#3379,0.96873629022557,0.685);
#273=CYLINDRICAL_SURFACE('',#3313,0.685);
#274=CYLINDRICAL_SURFACE('',#3324,0.685);
#275=CYLINDRICAL_SURFACE('',#3332,0.205);
#276=CYLINDRICAL_SURFACE('',#3334,0.25);
#277=CYLINDRICAL_SURFACE('',#3338,0.25);
#278=CYLINDRICAL_SURFACE('',#3342,0.33);
#279=CYLINDRICAL_SURFACE('',#3346,0.33);
#280=CYLINDRICAL_SURFACE('',#3350,0.205);
#281=CYLINDRICAL_SURFACE('',#3352,0.25);
#282=CYLINDRICAL_SURFACE('',#3356,0.25);
#283=CYLINDRICAL_SURFACE('',#3360,0.33);
#284=CYLINDRICAL_SURFACE('',#3364,0.33);
#285=CYLINDRICAL_SURFACE('',#3369,0.685);
#286=CYLINDRICAL_SURFACE('',#3382,0.685);
#287=CYLINDRICAL_SURFACE('',#3386,0.685);
#288=CYLINDRICAL_SURFACE('',#3397,0.515);
#289=CYLINDRICAL_SURFACE('',#3411,0.2);
#290=CYLINDRICAL_SURFACE('',#3413,0.685);
#291=CYLINDRICAL_SURFACE('',#3417,0.515);
#292=CYLINDRICAL_SURFACE('',#3431,0.2);
#293=CYLINDRICAL_SURFACE('',#3433,0.685);
#294=CYLINDRICAL_SURFACE('',#3437,0.515);
#295=CYLINDRICAL_SURFACE('',#3451,0.2);
#296=CYLINDRICAL_SURFACE('',#3453,0.685);
#297=CYLINDRICAL_SURFACE('',#3457,0.515);
#298=CYLINDRICAL_SURFACE('',#3471,0.2);
#299=CYLINDRICAL_SURFACE('',#3473,0.685);
#300=CYLINDRICAL_SURFACE('',#3477,0.205);
#301=CYLINDRICAL_SURFACE('',#3480,0.33);
#302=CYLINDRICAL_SURFACE('',#3483,0.33);
#303=CYLINDRICAL_SURFACE('',#3486,0.625);
#304=CYLINDRICAL_SURFACE('',#3491,0.625);
#305=CYLINDRICAL_SURFACE('',#3496,0.33);
#306=CYLINDRICAL_SURFACE('',#3498,0.33);
#307=CYLINDRICAL_SURFACE('',#3507,0.205);
#308=CYLINDRICAL_SURFACE('',#3510,0.33);
#309=CYLINDRICAL_SURFACE('',#3513,0.33);
#310=CYLINDRICAL_SURFACE('',#3516,0.625);
#311=CYLINDRICAL_SURFACE('',#3521,0.625);
#312=CYLINDRICAL_SURFACE('',#3526,0.33);
#313=CYLINDRICAL_SURFACE('',#3528,0.33);
#314=CYLINDRICAL_SURFACE('',#3540,0.46);
#315=CYLINDRICAL_SURFACE('',#3552,0.685);
#316=CYLINDRICAL_SURFACE('',#3553,0.685);
#317=CYLINDRICAL_SURFACE('',#3559,0.685);
#318=CYLINDRICAL_SURFACE('',#3573,0.43);
#319=CYLINDRICAL_SURFACE('',#3590,0.46);
#320=CYLINDRICAL_SURFACE('',#3594,0.525);
#321=CYLINDRICAL_SURFACE('',#3595,0.515);
#322=CYLINDRICAL_SURFACE('',#3599,0.2);
#323=CYLINDRICAL_SURFACE('',#3604,0.475);
#324=CYLINDRICAL_SURFACE('',#3608,0.355);
#325=CYLINDRICAL_SURFACE('',#3612,0.31);
#326=CYLINDRICAL_SURFACE('',#3618,0.2);
#327=CYLINDRICAL_SURFACE('',#3624,0.32);
#328=CYLINDRICAL_SURFACE('',#3627,0.6);
#329=CYLINDRICAL_SURFACE('',#3633,0.2942);
#330=FACE_OUTER_BOUND('',#516,.T.);
#331=FACE_OUTER_BOUND('',#517,.T.);
#332=FACE_OUTER_BOUND('',#518,.T.);
#333=FACE_OUTER_BOUND('',#519,.T.);
#334=FACE_OUTER_BOUND('',#520,.T.);
#335=FACE_OUTER_BOUND('',#521,.T.);
#336=FACE_OUTER_BOUND('',#522,.T.);
#337=FACE_OUTER_BOUND('',#523,.T.);
#338=FACE_OUTER_BOUND('',#524,.T.);
#339=FACE_OUTER_BOUND('',#525,.T.);
#340=FACE_OUTER_BOUND('',#526,.T.);
#341=FACE_OUTER_BOUND('',#527,.T.);
#342=FACE_OUTER_BOUND('',#529,.T.);
#343=FACE_OUTER_BOUND('',#530,.T.);
#344=FACE_OUTER_BOUND('',#532,.T.);
#345=FACE_OUTER_BOUND('',#533,.T.);
#346=FACE_OUTER_BOUND('',#534,.T.);
#347=FACE_OUTER_BOUND('',#535,.T.);
#348=FACE_OUTER_BOUND('',#536,.T.);
#349=FACE_OUTER_BOUND('',#537,.T.);
#350=FACE_OUTER_BOUND('',#538,.T.);
#351=FACE_OUTER_BOUND('',#540,.T.);
#352=FACE_OUTER_BOUND('',#541,.T.);
#353=FACE_OUTER_BOUND('',#543,.T.);
#354=FACE_OUTER_BOUND('',#544,.T.);
#355=FACE_OUTER_BOUND('',#547,.T.);
#356=FACE_OUTER_BOUND('',#548,.T.);
#357=FACE_OUTER_BOUND('',#549,.T.);
#358=FACE_OUTER_BOUND('',#550,.T.);
#359=FACE_OUTER_BOUND('',#551,.T.);
#360=FACE_OUTER_BOUND('',#552,.T.);
#361=FACE_OUTER_BOUND('',#553,.T.);
#362=FACE_OUTER_BOUND('',#554,.T.);
#363=FACE_OUTER_BOUND('',#556,.T.);
#364=FACE_OUTER_BOUND('',#557,.T.);
#365=FACE_OUTER_BOUND('',#559,.T.);
#366=FACE_OUTER_BOUND('',#564,.T.);
#367=FACE_OUTER_BOUND('',#571,.T.);
#368=FACE_OUTER_BOUND('',#572,.T.);
#369=FACE_OUTER_BOUND('',#574,.T.);
#370=FACE_OUTER_BOUND('',#576,.T.);
#371=FACE_OUTER_BOUND('',#577,.T.);
#372=FACE_OUTER_BOUND('',#578,.T.);
#373=FACE_OUTER_BOUND('',#579,.T.);
#374=FACE_OUTER_BOUND('',#580,.T.);
#375=FACE_OUTER_BOUND('',#581,.T.);
#376=FACE_OUTER_BOUND('',#582,.T.);
#377=FACE_OUTER_BOUND('',#584,.T.);
#378=FACE_OUTER_BOUND('',#585,.T.);
#379=FACE_OUTER_BOUND('',#586,.T.);
#380=FACE_OUTER_BOUND('',#588,.T.);
#381=FACE_OUTER_BOUND('',#589,.T.);
#382=FACE_OUTER_BOUND('',#591,.T.);
#383=FACE_OUTER_BOUND('',#593,.T.);
#384=FACE_OUTER_BOUND('',#594,.T.);
#385=FACE_OUTER_BOUND('',#595,.T.);
#386=FACE_OUTER_BOUND('',#596,.T.);
#387=FACE_OUTER_BOUND('',#597,.T.);
#388=FACE_OUTER_BOUND('',#598,.T.);
#389=FACE_OUTER_BOUND('',#599,.T.);
#390=FACE_OUTER_BOUND('',#601,.T.);
#391=FACE_OUTER_BOUND('',#602,.T.);
#392=FACE_OUTER_BOUND('',#603,.T.);
#393=FACE_OUTER_BOUND('',#605,.T.);
#394=FACE_OUTER_BOUND('',#606,.T.);
#395=FACE_OUTER_BOUND('',#608,.T.);
#396=FACE_OUTER_BOUND('',#610,.T.);
#397=FACE_OUTER_BOUND('',#611,.T.);
#398=FACE_OUTER_BOUND('',#612,.T.);
#399=FACE_OUTER_BOUND('',#613,.T.);
#400=FACE_OUTER_BOUND('',#614,.T.);
#401=FACE_OUTER_BOUND('',#615,.T.);
#402=FACE_OUTER_BOUND('',#616,.T.);
#403=FACE_OUTER_BOUND('',#618,.T.);
#404=FACE_OUTER_BOUND('',#619,.T.);
#405=FACE_OUTER_BOUND('',#620,.T.);
#406=FACE_OUTER_BOUND('',#622,.T.);
#407=FACE_OUTER_BOUND('',#623,.T.);
#408=FACE_OUTER_BOUND('',#625,.T.);
#409=FACE_OUTER_BOUND('',#627,.T.);
#410=FACE_OUTER_BOUND('',#628,.T.);
#411=FACE_OUTER_BOUND('',#629,.T.);
#412=FACE_OUTER_BOUND('',#630,.T.);
#413=FACE_OUTER_BOUND('',#631,.T.);
#414=FACE_OUTER_BOUND('',#632,.T.);
#415=FACE_OUTER_BOUND('',#633,.T.);
#416=FACE_OUTER_BOUND('',#635,.T.);
#417=FACE_OUTER_BOUND('',#636,.T.);
#418=FACE_OUTER_BOUND('',#637,.T.);
#419=FACE_OUTER_BOUND('',#639,.T.);
#420=FACE_OUTER_BOUND('',#640,.T.);
#421=FACE_OUTER_BOUND('',#641,.T.);
#422=FACE_OUTER_BOUND('',#642,.T.);
#423=FACE_OUTER_BOUND('',#643,.T.);
#424=FACE_OUTER_BOUND('',#645,.T.);
#425=FACE_OUTER_BOUND('',#646,.T.);
#426=FACE_OUTER_BOUND('',#648,.T.);
#427=FACE_OUTER_BOUND('',#649,.T.);
#428=FACE_OUTER_BOUND('',#650,.T.);
#429=FACE_OUTER_BOUND('',#651,.T.);
#430=FACE_OUTER_BOUND('',#652,.T.);
#431=FACE_OUTER_BOUND('',#653,.T.);
#432=FACE_OUTER_BOUND('',#654,.T.);
#433=FACE_OUTER_BOUND('',#660,.T.);
#434=FACE_OUTER_BOUND('',#666,.T.);
#435=FACE_OUTER_BOUND('',#667,.T.);
#436=FACE_OUTER_BOUND('',#668,.T.);
#437=FACE_OUTER_BOUND('',#669,.T.);
#438=FACE_OUTER_BOUND('',#670,.T.);
#439=FACE_OUTER_BOUND('',#672,.T.);
#440=FACE_OUTER_BOUND('',#673,.T.);
#441=FACE_OUTER_BOUND('',#675,.T.);
#442=FACE_OUTER_BOUND('',#676,.T.);
#443=FACE_OUTER_BOUND('',#677,.T.);
#444=FACE_OUTER_BOUND('',#678,.T.);
#445=FACE_OUTER_BOUND('',#679,.T.);
#446=FACE_OUTER_BOUND('',#680,.T.);
#447=FACE_OUTER_BOUND('',#681,.T.);
#448=FACE_OUTER_BOUND('',#687,.T.);
#449=FACE_OUTER_BOUND('',#693,.T.);
#450=FACE_OUTER_BOUND('',#695,.T.);
#451=FACE_OUTER_BOUND('',#696,.T.);
#452=FACE_OUTER_BOUND('',#698,.T.);
#453=FACE_OUTER_BOUND('',#700,.T.);
#454=FACE_OUTER_BOUND('',#701,.T.);
#455=FACE_OUTER_BOUND('',#702,.T.);
#456=FACE_OUTER_BOUND('',#703,.T.);
#457=FACE_OUTER_BOUND('',#704,.T.);
#458=FACE_OUTER_BOUND('',#705,.T.);
#459=FACE_OUTER_BOUND('',#706,.T.);
#460=FACE_OUTER_BOUND('',#707,.T.);
#461=FACE_OUTER_BOUND('',#708,.T.);
#462=FACE_OUTER_BOUND('',#709,.T.);
#463=FACE_OUTER_BOUND('',#711,.T.);
#464=FACE_OUTER_BOUND('',#712,.T.);
#465=FACE_OUTER_BOUND('',#713,.T.);
#466=FACE_OUTER_BOUND('',#715,.T.);
#467=FACE_OUTER_BOUND('',#716,.T.);
#468=FACE_OUTER_BOUND('',#717,.T.);
#469=FACE_OUTER_BOUND('',#718,.T.);
#470=FACE_OUTER_BOUND('',#719,.T.);
#471=FACE_OUTER_BOUND('',#720,.T.);
#472=FACE_OUTER_BOUND('',#721,.T.);
#473=FACE_OUTER_BOUND('',#722,.T.);
#474=FACE_OUTER_BOUND('',#723,.T.);
#475=FACE_OUTER_BOUND('',#725,.T.);
#476=FACE_OUTER_BOUND('',#727,.T.);
#477=FACE_OUTER_BOUND('',#729,.T.);
#478=FACE_OUTER_BOUND('',#730,.T.);
#479=FACE_OUTER_BOUND('',#731,.T.);
#480=FACE_OUTER_BOUND('',#732,.T.);
#481=FACE_OUTER_BOUND('',#733,.T.);
#482=FACE_OUTER_BOUND('',#734,.T.);
#483=FACE_OUTER_BOUND('',#735,.T.);
#484=FACE_OUTER_BOUND('',#737,.T.);
#485=FACE_OUTER_BOUND('',#738,.T.);
#486=FACE_OUTER_BOUND('',#740,.T.);
#487=FACE_OUTER_BOUND('',#741,.T.);
#488=FACE_OUTER_BOUND('',#742,.T.);
#489=FACE_OUTER_BOUND('',#744,.T.);
#490=FACE_OUTER_BOUND('',#745,.T.);
#491=FACE_OUTER_BOUND('',#747,.T.);
#492=FACE_OUTER_BOUND('',#748,.T.);
#493=FACE_OUTER_BOUND('',#750,.T.);
#494=FACE_OUTER_BOUND('',#751,.T.);
#495=FACE_OUTER_BOUND('',#753,.T.);
#496=FACE_OUTER_BOUND('',#754,.T.);
#497=FACE_OUTER_BOUND('',#755,.T.);
#498=FACE_OUTER_BOUND('',#756,.T.);
#499=FACE_OUTER_BOUND('',#757,.T.);
#500=FACE_OUTER_BOUND('',#758,.T.);
#501=FACE_OUTER_BOUND('',#759,.T.);
#502=FACE_OUTER_BOUND('',#760,.T.);
#503=FACE_OUTER_BOUND('',#762,.T.);
#504=FACE_OUTER_BOUND('',#764,.T.);
#505=FACE_OUTER_BOUND('',#765,.T.);
#506=FACE_OUTER_BOUND('',#766,.T.);
#507=FACE_OUTER_BOUND('',#767,.T.);
#508=FACE_OUTER_BOUND('',#768,.T.);
#509=FACE_OUTER_BOUND('',#769,.T.);
#510=FACE_OUTER_BOUND('',#770,.T.);
#511=FACE_OUTER_BOUND('',#771,.T.);
#512=FACE_OUTER_BOUND('',#772,.T.);
#513=FACE_OUTER_BOUND('',#773,.T.);
#514=FACE_OUTER_BOUND('',#774,.T.);
#515=FACE_OUTER_BOUND('',#775,.T.);
#516=EDGE_LOOP('',(#2044,#2045));
#517=EDGE_LOOP('',(#2046,#2047,#2048,#2049,#2050,#2051,#2052,#2053,#2054));
#518=EDGE_LOOP('',(#2055,#2056));
#519=EDGE_LOOP('',(#2057,#2058));
#520=EDGE_LOOP('',(#2059,#2060,#2061,#2062,#2063,#2064,#2065,#2066,#2067));
#521=EDGE_LOOP('',(#2068,#2069,#2070,#2071,#2072));
#522=EDGE_LOOP('',(#2073,#2074,#2075,#2076));
#523=EDGE_LOOP('',(#2077));
#524=EDGE_LOOP('',(#2078,#2079,#2080,#2081));
#525=EDGE_LOOP('',(#2082));
#526=EDGE_LOOP('',(#2083,#2084,#2085,#2086));
#527=EDGE_LOOP('',(#2087));
#528=EDGE_LOOP('',(#2088));
#529=EDGE_LOOP('',(#2089,#2090,#2091,#2092));
#530=EDGE_LOOP('',(#2093));
#531=EDGE_LOOP('',(#2094));
#532=EDGE_LOOP('',(#2095,#2096,#2097,#2098,#2099));
#533=EDGE_LOOP('',(#2100,#2101,#2102,#2103));
#534=EDGE_LOOP('',(#2104));
#535=EDGE_LOOP('',(#2105,#2106,#2107,#2108));
#536=EDGE_LOOP('',(#2109));
#537=EDGE_LOOP('',(#2110,#2111,#2112,#2113));
#538=EDGE_LOOP('',(#2114));
#539=EDGE_LOOP('',(#2115));
#540=EDGE_LOOP('',(#2116,#2117,#2118,#2119));
#541=EDGE_LOOP('',(#2120));
#542=EDGE_LOOP('',(#2121));
#543=EDGE_LOOP('',(#2122,#2123));
#544=EDGE_LOOP('',(#2124,#2125,#2126,#2127,#2128,#2129,#2130,#2131,#2132,
#2133,#2134,#2135,#2136,#2137,#2138,#2139,#2140,#2141,#2142,#2143,#2144,
#2145,#2146,#2147,#2148,#2149,#2150,#2151,#2152,#2153,#2154,#2155,#2156,
#2157,#2158,#2159));
#545=EDGE_LOOP('',(#2160,#2161));
#546=EDGE_LOOP('',(#2162,#2163));
#547=EDGE_LOOP('',(#2164,#2165));
#548=EDGE_LOOP('',(#2166,#2167,#2168,#2169,#2170,#2171,#2172,#2173,#2174));
#549=EDGE_LOOP('',(#2175,#2176));
#550=EDGE_LOOP('',(#2177,#2178,#2179,#2180,#2181,#2182,#2183,#2184,#2185));
#551=EDGE_LOOP('',(#2186,#2187));
#552=EDGE_LOOP('',(#2188,#2189));
#553=EDGE_LOOP('',(#2190,#2191,#2192,#2193));
#554=EDGE_LOOP('',(#2194,#2195,#2196,#2197));
#555=EDGE_LOOP('',(#2198));
#556=EDGE_LOOP('',(#2199,#2200,#2201,#2202));
#557=EDGE_LOOP('',(#2203,#2204,#2205,#2206));
#558=EDGE_LOOP('',(#2207));
#559=EDGE_LOOP('',(#2208,#2209,#2210,#2211));
#560=EDGE_LOOP('',(#2212));
#561=EDGE_LOOP('',(#2213));
#562=EDGE_LOOP('',(#2214));
#563=EDGE_LOOP('',(#2215));
#564=EDGE_LOOP('',(#2216,#2217,#2218,#2219));
#565=EDGE_LOOP('',(#2220));
#566=EDGE_LOOP('',(#2221));
#567=EDGE_LOOP('',(#2222));
#568=EDGE_LOOP('',(#2223));
#569=EDGE_LOOP('',(#2224));
#570=EDGE_LOOP('',(#2225));
#571=EDGE_LOOP('',(#2226,#2227,#2228,#2229));
#572=EDGE_LOOP('',(#2230));
#573=EDGE_LOOP('',(#2231));
#574=EDGE_LOOP('',(#2232,#2233,#2234,#2235,#2236,#2237));
#575=EDGE_LOOP('',(#2238));
#576=EDGE_LOOP('',(#2239,#2240,#2241,#2242));
#577=EDGE_LOOP('',(#2243,#2244,#2245,#2246));
#578=EDGE_LOOP('',(#2247,#2248,#2249,#2250));
#579=EDGE_LOOP('',(#2251,#2252,#2253,#2254));
#580=EDGE_LOOP('',(#2255,#2256,#2257,#2258));
#581=EDGE_LOOP('',(#2259,#2260,#2261,#2262));
#582=EDGE_LOOP('',(#2263,#2264,#2265,#2266,#2267,#2268));
#583=EDGE_LOOP('',(#2269));
#584=EDGE_LOOP('',(#2270,#2271,#2272,#2273));
#585=EDGE_LOOP('',(#2274,#2275,#2276,#2277));
#586=EDGE_LOOP('',(#2278));
#587=EDGE_LOOP('',(#2279));
#588=EDGE_LOOP('',(#2280,#2281,#2282,#2283));
#589=EDGE_LOOP('',(#2284));
#590=EDGE_LOOP('',(#2285));
#591=EDGE_LOOP('',(#2286,#2287,#2288,#2289,#2290,#2291));
#592=EDGE_LOOP('',(#2292));
#593=EDGE_LOOP('',(#2293,#2294,#2295,#2296));
#594=EDGE_LOOP('',(#2297,#2298,#2299,#2300));
#595=EDGE_LOOP('',(#2301,#2302,#2303,#2304));
#596=EDGE_LOOP('',(#2305,#2306,#2307,#2308));
#597=EDGE_LOOP('',(#2309,#2310,#2311,#2312));
#598=EDGE_LOOP('',(#2313,#2314,#2315,#2316));
#599=EDGE_LOOP('',(#2317,#2318,#2319,#2320,#2321,#2322));
#600=EDGE_LOOP('',(#2323));
#601=EDGE_LOOP('',(#2324,#2325,#2326,#2327));
#602=EDGE_LOOP('',(#2328,#2329,#2330,#2331));
#603=EDGE_LOOP('',(#2332));
#604=EDGE_LOOP('',(#2333));
#605=EDGE_LOOP('',(#2334,#2335,#2336,#2337));
#606=EDGE_LOOP('',(#2338));
#607=EDGE_LOOP('',(#2339));
#608=EDGE_LOOP('',(#2340,#2341,#2342,#2343,#2344,#2345));
#609=EDGE_LOOP('',(#2346));
#610=EDGE_LOOP('',(#2347,#2348,#2349,#2350));
#611=EDGE_LOOP('',(#2351,#2352,#2353,#2354));
#612=EDGE_LOOP('',(#2355,#2356,#2357,#2358));
#613=EDGE_LOOP('',(#2359,#2360,#2361,#2362));
#614=EDGE_LOOP('',(#2363,#2364,#2365,#2366));
#615=EDGE_LOOP('',(#2367,#2368,#2369,#2370));
#616=EDGE_LOOP('',(#2371,#2372,#2373,#2374,#2375,#2376));
#617=EDGE_LOOP('',(#2377));
#618=EDGE_LOOP('',(#2378,#2379,#2380,#2381));
#619=EDGE_LOOP('',(#2382,#2383,#2384,#2385));
#620=EDGE_LOOP('',(#2386));
#621=EDGE_LOOP('',(#2387));
#622=EDGE_LOOP('',(#2388,#2389,#2390,#2391));
#623=EDGE_LOOP('',(#2392));
#624=EDGE_LOOP('',(#2393));
#625=EDGE_LOOP('',(#2394,#2395,#2396,#2397,#2398,#2399));
#626=EDGE_LOOP('',(#2400));
#627=EDGE_LOOP('',(#2401,#2402,#2403,#2404));
#628=EDGE_LOOP('',(#2405,#2406,#2407,#2408));
#629=EDGE_LOOP('',(#2409,#2410,#2411,#2412));
#630=EDGE_LOOP('',(#2413,#2414,#2415,#2416));
#631=EDGE_LOOP('',(#2417,#2418,#2419,#2420));
#632=EDGE_LOOP('',(#2421,#2422,#2423,#2424));
#633=EDGE_LOOP('',(#2425,#2426,#2427,#2428,#2429,#2430));
#634=EDGE_LOOP('',(#2431));
#635=EDGE_LOOP('',(#2432,#2433,#2434,#2435));
#636=EDGE_LOOP('',(#2436,#2437,#2438,#2439));
#637=EDGE_LOOP('',(#2440));
#638=EDGE_LOOP('',(#2441));
#639=EDGE_LOOP('',(#2442,#2443,#2444,#2445));
#640=EDGE_LOOP('',(#2446,#2447,#2448,#2449));
#641=EDGE_LOOP('',(#2450,#2451,#2452,#2453));
#642=EDGE_LOOP('',(#2454,#2455,#2456,#2457));
#643=EDGE_LOOP('',(#2458));
#644=EDGE_LOOP('',(#2459));
#645=EDGE_LOOP('',(#2460,#2461,#2462,#2463));
#646=EDGE_LOOP('',(#2464));
#647=EDGE_LOOP('',(#2465));
#648=EDGE_LOOP('',(#2466,#2467,#2468,#2469));
#649=EDGE_LOOP('',(#2470,#2471,#2472,#2473));
#650=EDGE_LOOP('',(#2474,#2475,#2476,#2477));
#651=EDGE_LOOP('',(#2478,#2479,#2480,#2481));
#652=EDGE_LOOP('',(#2482,#2483,#2484,#2485));
#653=EDGE_LOOP('',(#2486,#2487,#2488,#2489));
#654=EDGE_LOOP('',(#2490,#2491,#2492,#2493));
#655=EDGE_LOOP('',(#2494));
#656=EDGE_LOOP('',(#2495));
#657=EDGE_LOOP('',(#2496));
#658=EDGE_LOOP('',(#2497));
#659=EDGE_LOOP('',(#2498));
#660=EDGE_LOOP('',(#2499,#2500,#2501,#2502));
#661=EDGE_LOOP('',(#2503));
#662=EDGE_LOOP('',(#2504));
#663=EDGE_LOOP('',(#2505));
#664=EDGE_LOOP('',(#2506));
#665=EDGE_LOOP('',(#2507));
#666=EDGE_LOOP('',(#2508,#2509,#2510,#2511));
#667=EDGE_LOOP('',(#2512,#2513,#2514,#2515));
#668=EDGE_LOOP('',(#2516,#2517,#2518,#2519));
#669=EDGE_LOOP('',(#2520,#2521,#2522,#2523));
#670=EDGE_LOOP('',(#2524));
#671=EDGE_LOOP('',(#2525));
#672=EDGE_LOOP('',(#2526,#2527,#2528,#2529));
#673=EDGE_LOOP('',(#2530));
#674=EDGE_LOOP('',(#2531));
#675=EDGE_LOOP('',(#2532,#2533,#2534,#2535));
#676=EDGE_LOOP('',(#2536,#2537,#2538,#2539));
#677=EDGE_LOOP('',(#2540,#2541,#2542,#2543));
#678=EDGE_LOOP('',(#2544,#2545,#2546,#2547));
#679=EDGE_LOOP('',(#2548,#2549,#2550,#2551));
#680=EDGE_LOOP('',(#2552,#2553,#2554,#2555));
#681=EDGE_LOOP('',(#2556,#2557,#2558,#2559));
#682=EDGE_LOOP('',(#2560));
#683=EDGE_LOOP('',(#2561));
#684=EDGE_LOOP('',(#2562));
#685=EDGE_LOOP('',(#2563));
#686=EDGE_LOOP('',(#2564));
#687=EDGE_LOOP('',(#2565,#2566,#2567,#2568));
#688=EDGE_LOOP('',(#2569));
#689=EDGE_LOOP('',(#2570));
#690=EDGE_LOOP('',(#2571));
#691=EDGE_LOOP('',(#2572));
#692=EDGE_LOOP('',(#2573));
#693=EDGE_LOOP('',(#2574));
#694=EDGE_LOOP('',(#2575));
#695=EDGE_LOOP('',(#2576,#2577,#2578,#2579));
#696=EDGE_LOOP('',(#2580,#2581,#2582,#2583,#2584,#2585));
#697=EDGE_LOOP('',(#2586));
#698=EDGE_LOOP('',(#2587,#2588,#2589,#2590,#2591,#2592));
#699=EDGE_LOOP('',(#2593));
#700=EDGE_LOOP('',(#2594,#2595,#2596,#2597));
#701=EDGE_LOOP('',(#2598,#2599,#2600,#2601));
#702=EDGE_LOOP('',(#2602,#2603,#2604,#2605));
#703=EDGE_LOOP('',(#2606,#2607,#2608,#2609));
#704=EDGE_LOOP('',(#2610,#2611,#2612,#2613));
#705=EDGE_LOOP('',(#2614,#2615,#2616,#2617));
#706=EDGE_LOOP('',(#2618,#2619,#2620,#2621));
#707=EDGE_LOOP('',(#2622,#2623,#2624,#2625));
#708=EDGE_LOOP('',(#2626,#2627,#2628,#2629));
#709=EDGE_LOOP('',(#2630));
#710=EDGE_LOOP('',(#2631));
#711=EDGE_LOOP('',(#2632,#2633,#2634,#2635));
#712=EDGE_LOOP('',(#2636));
#713=EDGE_LOOP('',(#2637,#2638,#2639,#2640,#2641,#2642));
#714=EDGE_LOOP('',(#2643));
#715=EDGE_LOOP('',(#2644,#2645,#2646,#2647));
#716=EDGE_LOOP('',(#2648,#2649,#2650,#2651));
#717=EDGE_LOOP('',(#2652,#2653,#2654,#2655));
#718=EDGE_LOOP('',(#2656,#2657,#2658,#2659));
#719=EDGE_LOOP('',(#2660,#2661,#2662,#2663));
#720=EDGE_LOOP('',(#2664,#2665,#2666,#2667));
#721=EDGE_LOOP('',(#2668,#2669,#2670,#2671,#2672,#2673));
#722=EDGE_LOOP('',(#2674,#2675,#2676,#2677));
#723=EDGE_LOOP('',(#2678));
#724=EDGE_LOOP('',(#2679));
#725=EDGE_LOOP('',(#2680,#2681,#2682,#2683,#2684,#2685));
#726=EDGE_LOOP('',(#2686));
#727=EDGE_LOOP('',(#2687,#2688,#2689,#2690,#2691,#2692));
#728=EDGE_LOOP('',(#2693));
#729=EDGE_LOOP('',(#2694,#2695,#2696,#2697));
#730=EDGE_LOOP('',(#2698,#2699,#2700,#2701));
#731=EDGE_LOOP('',(#2702,#2703,#2704,#2705));
#732=EDGE_LOOP('',(#2706,#2707,#2708,#2709));
#733=EDGE_LOOP('',(#2710,#2711,#2712,#2713));
#734=EDGE_LOOP('',(#2714,#2715,#2716,#2717));
#735=EDGE_LOOP('',(#2718));
#736=EDGE_LOOP('',(#2719));
#737=EDGE_LOOP('',(#2720,#2721,#2722,#2723));
#738=EDGE_LOOP('',(#2724));
#739=EDGE_LOOP('',(#2725));
#740=EDGE_LOOP('',(#2726,#2727,#2728,#2729));
#741=EDGE_LOOP('',(#2730,#2731,#2732,#2733));
#742=EDGE_LOOP('',(#2734));
#743=EDGE_LOOP('',(#2735));
#744=EDGE_LOOP('',(#2736,#2737,#2738,#2739));
#745=EDGE_LOOP('',(#2740));
#746=EDGE_LOOP('',(#2741));
#747=EDGE_LOOP('',(#2742,#2743,#2744,#2745));
#748=EDGE_LOOP('',(#2746));
#749=EDGE_LOOP('',(#2747));
#750=EDGE_LOOP('',(#2748,#2749,#2750,#2751));
#751=EDGE_LOOP('',(#2752));
#752=EDGE_LOOP('',(#2753));
#753=EDGE_LOOP('',(#2754,#2755,#2756,#2757));
#754=EDGE_LOOP('',(#2758));
#755=EDGE_LOOP('',(#2759,#2760,#2761,#2762));
#756=EDGE_LOOP('',(#2763,#2764,#2765,#2766));
#757=EDGE_LOOP('',(#2767));
#758=EDGE_LOOP('',(#2768,#2769,#2770,#2771));
#759=EDGE_LOOP('',(#2772,#2773,#2774,#2775));
#760=EDGE_LOOP('',(#2776));
#761=EDGE_LOOP('',(#2777));
#762=EDGE_LOOP('',(#2778));
#763=EDGE_LOOP('',(#2779));
#764=EDGE_LOOP('',(#2780,#2781,#2782,#2783));
#765=EDGE_LOOP('',(#2784,#2785,#2786,#2787));
#766=EDGE_LOOP('',(#2788));
#767=EDGE_LOOP('',(#2789,#2790,#2791,#2792,#2793,#2794,#2795,#2796,#2797));
#768=EDGE_LOOP('',(#2798,#2799,#2800,#2801));
#769=EDGE_LOOP('',(#2802,#2803,#2804,#2805));
#770=EDGE_LOOP('',(#2806,#2807,#2808,#2809));
#771=EDGE_LOOP('',(#2810,#2811,#2812,#2813));
#772=EDGE_LOOP('',(#2814,#2815,#2816,#2817));
#773=EDGE_LOOP('',(#2818,#2819,#2820,#2821));
#774=EDGE_LOOP('',(#2822));
#775=EDGE_LOOP('',(#2823,#2824,#2825,#2826,#2827,#2828));
#776=EDGE_LOOP('',(#2829));
#777=CIRCLE('',#3312,0.685);
#778=CIRCLE('',#3317,0.685);
#779=CIRCLE('',#3319,0.685);
#780=CIRCLE('',#3321,0.685);
#781=CIRCLE('',#3323,0.685);
#782=CIRCLE('',#3326,0.685);
#783=CIRCLE('',#3328,0.685);
#784=CIRCLE('',#3331,0.685);
#785=CIRCLE('',#3333,0.205);
#786=CIRCLE('',#3335,0.25);
#787=CIRCLE('',#3336,0.25);
#788=CIRCLE('',#3339,0.25);
#789=CIRCLE('',#3340,0.25);
#790=CIRCLE('',#3343,0.33);
#791=CIRCLE('',#3344,0.33);
#792=CIRCLE('',#3347,0.33);
#793=CIRCLE('',#3348,0.33);
#794=CIRCLE('',#3351,0.205);
#795=CIRCLE('',#3353,0.25);
#796=CIRCLE('',#3354,0.25);
#797=CIRCLE('',#3357,0.25);
#798=CIRCLE('',#3358,0.25);
#799=CIRCLE('',#3361,0.33);
#800=CIRCLE('',#3362,0.33);
#801=CIRCLE('',#3365,0.33);
#802=CIRCLE('',#3366,0.33);
#803=CIRCLE('',#3370,0.685);
#804=CIRCLE('',#3375,0.685);
#805=CIRCLE('',#3381,0.685);
#806=CIRCLE('',#3383,0.685);
#807=CIRCLE('',#3385,0.685);
#808=CIRCLE('',#3387,0.685);
#809=CIRCLE('',#3398,0.515);
#810=CIRCLE('',#3399,0.515);
#811=CIRCLE('',#3401,0.2);
#812=CIRCLE('',#3403,0.685);
#813=CIRCLE('',#3412,0.2);
#814=CIRCLE('',#3414,0.685);
#815=CIRCLE('',#3418,0.515);
#816=CIRCLE('',#3419,0.515);
#817=CIRCLE('',#3421,0.2);
#818=CIRCLE('',#3423,0.685);
#819=CIRCLE('',#3432,0.2);
#820=CIRCLE('',#3434,0.685);
#821=CIRCLE('',#3438,0.515);
#822=CIRCLE('',#3439,0.515);
#823=CIRCLE('',#3441,0.2);
#824=CIRCLE('',#3443,0.685);
#825=CIRCLE('',#3452,0.2);
#826=CIRCLE('',#3454,0.685);
#827=CIRCLE('',#3458,0.515);
#828=CIRCLE('',#3459,0.515);
#829=CIRCLE('',#3461,0.2);
#830=CIRCLE('',#3463,0.685);
#831=CIRCLE('',#3472,0.2);
#832=CIRCLE('',#3474,0.685);
#833=CIRCLE('',#3478,0.205);
#834=CIRCLE('',#3479,0.205);
#835=CIRCLE('',#3481,0.33);
#836=CIRCLE('',#3482,0.33);
#837=CIRCLE('',#3484,0.33);
#838=CIRCLE('',#3485,0.33);
#839=CIRCLE('',#3487,0.625);
#840=CIRCLE('',#3488,0.625);
#841=CIRCLE('',#3490,0.33);
#842=CIRCLE('',#3492,0.625);
#843=CIRCLE('',#3493,0.625);
#844=CIRCLE('',#3495,0.33);
#845=CIRCLE('',#3497,0.33);
#846=CIRCLE('',#3499,0.33);
#847=CIRCLE('',#3508,0.205);
#848=CIRCLE('',#3509,0.205);
#849=CIRCLE('',#3511,0.33);
#850=CIRCLE('',#3512,0.33);
#851=CIRCLE('',#3514,0.33);
#852=CIRCLE('',#3515,0.33);
#853=CIRCLE('',#3517,0.625);
#854=CIRCLE('',#3518,0.625);
#855=CIRCLE('',#3520,0.33);
#856=CIRCLE('',#3522,0.625);
#857=CIRCLE('',#3523,0.625);
#858=CIRCLE('',#3525,0.33);
#859=CIRCLE('',#3527,0.33);
#860=CIRCLE('',#3529,0.33);
#861=CIRCLE('',#3538,0.685);
#862=CIRCLE('',#3539,0.46);
#863=CIRCLE('',#3541,0.46);
#864=CIRCLE('',#3543,0.685);
#865=CIRCLE('',#3545,0.685);
#866=CIRCLE('',#3554,0.685);
#867=CIRCLE('',#3556,0.605);
#868=CIRCLE('',#3560,0.685);
#869=CIRCLE('',#3561,0.685);
#870=CIRCLE('',#3574,0.43);
#871=CIRCLE('',#3575,0.43);
#872=CIRCLE('',#3577,0.2);
#873=CIRCLE('',#3579,0.525);
#874=CIRCLE('',#3581,0.515);
#875=CIRCLE('',#3589,0.46);
#876=CIRCLE('',#3591,0.46);
#877=CIRCLE('',#3593,0.525);
#878=CIRCLE('',#3596,0.515);
#879=CIRCLE('',#3598,0.2);
#880=CIRCLE('',#3602,0.475);
#881=CIRCLE('',#3603,0.31);
#882=CIRCLE('',#3605,0.475);
#883=CIRCLE('',#3607,0.355);
#884=CIRCLE('',#3609,0.355);
#885=CIRCLE('',#3611,0.31);
#886=CIRCLE('',#3617,0.2);
#887=CIRCLE('',#3619,0.2);
#888=CIRCLE('',#3621,0.14);
#889=CIRCLE('',#3625,0.32);
#890=CIRCLE('',#3626,0.32);
#891=CIRCLE('',#3628,0.6);
#892=CIRCLE('',#3629,0.6);
#893=CIRCLE('',#3634,0.2942);
#894=CIRCLE('',#3635,0.2942);
#895=CIRCLE('',#3637,0.24);
#896=CIRCLE('',#3640,0.475);
#897=LINE('',#4650,#1144);
#898=LINE('',#4660,#1145);
#899=LINE('',#4668,#1146);
#900=LINE('',#4673,#1147);
#901=LINE('',#4680,#1148);
#902=LINE('',#4695,#1149);
#903=LINE('',#4737,#1150);
#904=LINE('',#4744,#1151);
#905=LINE('',#4751,#1152);
#906=LINE('',#4758,#1153);
#907=LINE('',#4765,#1154);
#908=LINE('',#4807,#1155);
#909=LINE('',#4814,#1156);
#910=LINE('',#4821,#1157);
#911=LINE('',#4828,#1158);
#912=LINE('',#4832,#1159);
#913=LINE('',#4836,#1160);
#914=LINE('',#4837,#1161);
#915=LINE('',#4839,#1162);
#916=LINE('',#4843,#1163);
#917=LINE('',#4847,#1164);
#918=LINE('',#4851,#1165);
#919=LINE('',#4854,#1166);
#920=LINE('',#4856,#1167);
#921=LINE('',#4862,#1168);
#922=LINE('',#4867,#1169);
#923=LINE('',#4873,#1170);
#924=LINE('',#4880,#1171);
#925=LINE('',#4882,#1172);
#926=LINE('',#4884,#1173);
#927=LINE('',#4885,#1174);
#928=LINE('',#4888,#1175);
#929=LINE('',#4890,#1176);
#930=LINE('',#4891,#1177);
#931=LINE('',#4894,#1178);
#932=LINE('',#4896,#1179);
#933=LINE('',#4897,#1180);
#934=LINE('',#4899,#1181);
#935=LINE('',#4900,#1182);
#936=LINE('',#4908,#1183);
#937=LINE('',#4916,#1184);
#938=LINE('',#4918,#1185);
#939=LINE('',#4920,#1186);
#940=LINE('',#4922,#1187);
#941=LINE('',#4924,#1188);
#942=LINE('',#4925,#1189);
#943=LINE('',#4930,#1190);
#944=LINE('',#4932,#1191);
#945=LINE('',#4933,#1192);
#946=LINE('',#4936,#1193);
#947=LINE('',#4937,#1194);
#948=LINE('',#4940,#1195);
#949=LINE('',#4941,#1196);
#950=LINE('',#4944,#1197);
#951=LINE('',#4945,#1198);
#952=LINE('',#4948,#1199);
#953=LINE('',#4949,#1200);
#954=LINE('',#4951,#1201);
#955=LINE('',#4955,#1202);
#956=LINE('',#4959,#1203);
#957=LINE('',#4967,#1204);
#958=LINE('',#4975,#1205);
#959=LINE('',#4977,#1206);
#960=LINE('',#4979,#1207);
#961=LINE('',#4981,#1208);
#962=LINE('',#4983,#1209);
#963=LINE('',#4984,#1210);
#964=LINE('',#4989,#1211);
#965=LINE('',#4991,#1212);
#966=LINE('',#4992,#1213);
#967=LINE('',#4995,#1214);
#968=LINE('',#4996,#1215);
#969=LINE('',#4999,#1216);
#970=LINE('',#5000,#1217);
#971=LINE('',#5003,#1218);
#972=LINE('',#5004,#1219);
#973=LINE('',#5007,#1220);
#974=LINE('',#5008,#1221);
#975=LINE('',#5010,#1222);
#976=LINE('',#5014,#1223);
#977=LINE('',#5018,#1224);
#978=LINE('',#5026,#1225);
#979=LINE('',#5034,#1226);
#980=LINE('',#5036,#1227);
#981=LINE('',#5038,#1228);
#982=LINE('',#5040,#1229);
#983=LINE('',#5042,#1230);
#984=LINE('',#5043,#1231);
#985=LINE('',#5048,#1232);
#986=LINE('',#5050,#1233);
#987=LINE('',#5051,#1234);
#988=LINE('',#5054,#1235);
#989=LINE('',#5055,#1236);
#990=LINE('',#5058,#1237);
#991=LINE('',#5059,#1238);
#992=LINE('',#5062,#1239);
#993=LINE('',#5063,#1240);
#994=LINE('',#5066,#1241);
#995=LINE('',#5067,#1242);
#996=LINE('',#5069,#1243);
#997=LINE('',#5073,#1244);
#998=LINE('',#5077,#1245);
#999=LINE('',#5085,#1246);
#1000=LINE('',#5093,#1247);
#1001=LINE('',#5095,#1248);
#1002=LINE('',#5097,#1249);
#1003=LINE('',#5099,#1250);
#1004=LINE('',#5101,#1251);
#1005=LINE('',#5102,#1252);
#1006=LINE('',#5107,#1253);
#1007=LINE('',#5109,#1254);
#1008=LINE('',#5110,#1255);
#1009=LINE('',#5113,#1256);
#1010=LINE('',#5114,#1257);
#1011=LINE('',#5117,#1258);
#1012=LINE('',#5118,#1259);
#1013=LINE('',#5121,#1260);
#1014=LINE('',#5122,#1261);
#1015=LINE('',#5125,#1262);
#1016=LINE('',#5126,#1263);
#1017=LINE('',#5128,#1264);
#1018=LINE('',#5132,#1265);
#1019=LINE('',#5136,#1266);
#1020=LINE('',#5144,#1267);
#1021=LINE('',#5150,#1268);
#1022=LINE('',#5156,#1269);
#1023=LINE('',#5162,#1270);
#1024=LINE('',#5171,#1271);
#1025=LINE('',#5178,#1272);
#1026=LINE('',#5182,#1273);
#1027=LINE('',#5187,#1274);
#1028=LINE('',#5189,#1275);
#1029=LINE('',#5191,#1276);
#1030=LINE('',#5192,#1277);
#1031=LINE('',#5195,#1278);
#1032=LINE('',#5197,#1279);
#1033=LINE('',#5198,#1280);
#1034=LINE('',#5201,#1281);
#1035=LINE('',#5203,#1282);
#1036=LINE('',#5204,#1283);
#1037=LINE('',#5206,#1284);
#1038=LINE('',#5207,#1285);
#1039=LINE('',#5215,#1286);
#1040=LINE('',#5221,#1287);
#1041=LINE('',#5227,#1288);
#1042=LINE('',#5233,#1289);
#1043=LINE('',#5242,#1290);
#1044=LINE('',#5249,#1291);
#1045=LINE('',#5253,#1292);
#1046=LINE('',#5258,#1293);
#1047=LINE('',#5260,#1294);
#1048=LINE('',#5262,#1295);
#1049=LINE('',#5263,#1296);
#1050=LINE('',#5266,#1297);
#1051=LINE('',#5268,#1298);
#1052=LINE('',#5269,#1299);
#1053=LINE('',#5272,#1300);
#1054=LINE('',#5274,#1301);
#1055=LINE('',#5275,#1302);
#1056=LINE('',#5277,#1303);
#1057=LINE('',#5278,#1304);
#1058=LINE('',#5290,#1305);
#1059=LINE('',#5294,#1306);
#1060=LINE('',#5296,#1307);
#1061=LINE('',#5298,#1308);
#1062=LINE('',#5300,#1309);
#1063=LINE('',#5302,#1310);
#1064=LINE('',#5303,#1311);
#1065=LINE('',#5309,#1312);
#1066=LINE('',#5311,#1313);
#1067=LINE('',#5313,#1314);
#1068=LINE('',#5315,#1315);
#1069=LINE('',#5317,#1316);
#1070=LINE('',#5318,#1317);
#1071=LINE('',#5322,#1318);
#1072=LINE('',#5323,#1319);
#1073=LINE('',#5325,#1320);
#1074=LINE('',#5327,#1321);
#1075=LINE('',#5329,#1322);
#1076=LINE('',#5331,#1323);
#1077=LINE('',#5334,#1324);
#1078=LINE('',#5338,#1325);
#1079=LINE('',#5342,#1326);
#1080=LINE('',#5349,#1327);
#1081=LINE('',#5355,#1328);
#1082=LINE('',#5357,#1329);
#1083=LINE('',#5359,#1330);
#1084=LINE('',#5361,#1331);
#1085=LINE('',#5363,#1332);
#1086=LINE('',#5364,#1333);
#1087=LINE('',#5367,#1334);
#1088=LINE('',#5369,#1335);
#1089=LINE('',#5370,#1336);
#1090=LINE('',#5373,#1337);
#1091=LINE('',#5374,#1338);
#1092=LINE('',#5377,#1339);
#1093=LINE('',#5378,#1340);
#1094=LINE('',#5381,#1341);
#1095=LINE('',#5382,#1342);
#1096=LINE('',#5385,#1343);
#1097=LINE('',#5386,#1344);
#1098=LINE('',#5388,#1345);
#1099=LINE('',#5396,#1346);
#1100=LINE('',#5404,#1347);
#1101=LINE('',#5406,#1348);
#1102=LINE('',#5408,#1349);
#1103=LINE('',#5410,#1350);
#1104=LINE('',#5412,#1351);
#1105=LINE('',#5413,#1352);
#1106=LINE('',#5419,#1353);
#1107=LINE('',#5421,#1354);
#1108=LINE('',#5423,#1355);
#1109=LINE('',#5425,#1356);
#1110=LINE('',#5427,#1357);
#1111=LINE('',#5428,#1358);
#1112=LINE('',#5432,#1359);
#1113=LINE('',#5433,#1360);
#1114=LINE('',#5435,#1361);
#1115=LINE('',#5437,#1362);
#1116=LINE('',#5439,#1363);
#1117=LINE('',#5441,#1364);
#1118=LINE('',#5448,#1365);
#1119=LINE('',#5454,#1366);
#1120=LINE('',#5458,#1367);
#1121=LINE('',#5463,#1368);
#1122=LINE('',#5473,#1369);
#1123=LINE('',#5480,#1370);
#1124=LINE('',#5485,#1371);
#1125=LINE('',#5495,#1372);
#1126=LINE('',#5499,#1373);
#1127=LINE('',#5506,#1374);
#1128=LINE('',#5512,#1375);
#1129=LINE('',#5521,#1376);
#1130=LINE('',#5526,#1377);
#1131=LINE('',#5532,#1378);
#1132=LINE('',#5558,#1379);
#1133=LINE('',#5560,#1380);
#1134=LINE('',#5561,#1381);
#1135=LINE('',#5564,#1382);
#1136=LINE('',#5565,#1383);
#1137=LINE('',#5568,#1384);
#1138=LINE('',#5569,#1385);
#1139=LINE('',#5572,#1386);
#1140=LINE('',#5573,#1387);
#1141=LINE('',#5576,#1388);
#1142=LINE('',#5577,#1389);
#1143=LINE('',#5579,#1390);
#1144=VECTOR('',#3678,1.);
#1145=VECTOR('',#3689,0.685);
#1146=VECTOR('',#3698,1.);
#1147=VECTOR('',#3703,1.);
#1148=VECTOR('',#3710,0.685);
#1149=VECTOR('',#3727,0.205);
#1150=VECTOR('',#3732,0.25);
#1151=VECTOR('',#3741,0.25);
#1152=VECTOR('',#3750,0.33);
#1153=VECTOR('',#3759,0.33);
#1154=VECTOR('',#3768,0.205);
#1155=VECTOR('',#3773,0.25);
#1156=VECTOR('',#3782,0.25);
#1157=VECTOR('',#3791,0.33);
#1158=VECTOR('',#3800,0.33);
#1159=VECTOR('',#3807,1.);
#1160=VECTOR('',#3812,0.685);
#1161=VECTOR('',#3813,1.);
#1162=VECTOR('',#3814,0.685);
#1163=VECTOR('',#3817,1.);
#1164=VECTOR('',#3820,0.685);
#1165=VECTOR('',#3823,1.);
#1166=VECTOR('',#3826,0.685);
#1167=VECTOR('',#3827,0.685);
#1168=VECTOR('',#3838,1.);
#1169=VECTOR('',#3845,0.685);
#1170=VECTOR('',#3854,0.685);
#1171=VECTOR('',#3863,1.);
#1172=VECTOR('',#3864,1.);
#1173=VECTOR('',#3865,1.);
#1174=VECTOR('',#3866,1.);
#1175=VECTOR('',#3869,1.);
#1176=VECTOR('',#3870,1.);
#1177=VECTOR('',#3871,1.);
#1178=VECTOR('',#3874,1.);
#1179=VECTOR('',#3875,1.);
#1180=VECTOR('',#3876,1.);
#1181=VECTOR('',#3879,1.);
#1182=VECTOR('',#3880,1.);
#1183=VECTOR('',#3891,0.515);
#1184=VECTOR('',#3900,1.);
#1185=VECTOR('',#3901,1.);
#1186=VECTOR('',#3902,1.);
#1187=VECTOR('',#3903,1.);
#1188=VECTOR('',#3904,1.);
#1189=VECTOR('',#3905,1.);
#1190=VECTOR('',#3910,1.);
#1191=VECTOR('',#3911,1.);
#1192=VECTOR('',#3912,1.);
#1193=VECTOR('',#3915,1.);
#1194=VECTOR('',#3916,1.);
#1195=VECTOR('',#3919,1.);
#1196=VECTOR('',#3920,1.);
#1197=VECTOR('',#3923,1.);
#1198=VECTOR('',#3924,1.);
#1199=VECTOR('',#3927,1.);
#1200=VECTOR('',#3928,1.);
#1201=VECTOR('',#3931,1.);
#1202=VECTOR('',#3936,0.2);
#1203=VECTOR('',#3941,0.685);
#1204=VECTOR('',#3952,0.515);
#1205=VECTOR('',#3961,1.);
#1206=VECTOR('',#3962,1.);
#1207=VECTOR('',#3963,1.);
#1208=VECTOR('',#3964,1.);
#1209=VECTOR('',#3965,1.);
#1210=VECTOR('',#3966,1.);
#1211=VECTOR('',#3971,1.);
#1212=VECTOR('',#3972,1.);
#1213=VECTOR('',#3973,1.);
#1214=VECTOR('',#3976,1.);
#1215=VECTOR('',#3977,1.);
#1216=VECTOR('',#3980,1.);
#1217=VECTOR('',#3981,1.);
#1218=VECTOR('',#3984,1.);
#1219=VECTOR('',#3985,1.);
#1220=VECTOR('',#3988,1.);
#1221=VECTOR('',#3989,1.);
#1222=VECTOR('',#3992,1.);
#1223=VECTOR('',#3997,0.2);
#1224=VECTOR('',#4002,0.685);
#1225=VECTOR('',#4013,0.515);
#1226=VECTOR('',#4022,1.);
#1227=VECTOR('',#4023,1.);
#1228=VECTOR('',#4024,1.);
#1229=VECTOR('',#4025,1.);
#1230=VECTOR('',#4026,1.);
#1231=VECTOR('',#4027,1.);
#1232=VECTOR('',#4032,1.);
#1233=VECTOR('',#4033,1.);
#1234=VECTOR('',#4034,1.);
#1235=VECTOR('',#4037,1.);
#1236=VECTOR('',#4038,1.);
#1237=VECTOR('',#4041,1.);
#1238=VECTOR('',#4042,1.);
#1239=VECTOR('',#4045,1.);
#1240=VECTOR('',#4046,1.);
#1241=VECTOR('',#4049,1.);
#1242=VECTOR('',#4050,1.);
#1243=VECTOR('',#4053,1.);
#1244=VECTOR('',#4058,0.2);
#1245=VECTOR('',#4063,0.685);
#1246=VECTOR('',#4074,0.515);
#1247=VECTOR('',#4083,1.);
#1248=VECTOR('',#4084,1.);
#1249=VECTOR('',#4085,1.);
#1250=VECTOR('',#4086,1.);
#1251=VECTOR('',#4087,1.);
#1252=VECTOR('',#4088,1.);
#1253=VECTOR('',#4093,1.);
#1254=VECTOR('',#4094,1.);
#1255=VECTOR('',#4095,1.);
#1256=VECTOR('',#4098,1.);
#1257=VECTOR('',#4099,1.);
#1258=VECTOR('',#4102,1.);
#1259=VECTOR('',#4103,1.);
#1260=VECTOR('',#4106,1.);
#1261=VECTOR('',#4107,1.);
#1262=VECTOR('',#4110,1.);
#1263=VECTOR('',#4111,1.);
#1264=VECTOR('',#4114,1.);
#1265=VECTOR('',#4119,0.2);
#1266=VECTOR('',#4124,0.685);
#1267=VECTOR('',#4135,0.205);
#1268=VECTOR('',#4142,0.33);
#1269=VECTOR('',#4149,0.33);
#1270=VECTOR('',#4156,0.625);
#1271=VECTOR('',#4167,0.625);
#1272=VECTOR('',#4176,0.33);
#1273=VECTOR('',#4181,0.33);
#1274=VECTOR('',#4186,1.);
#1275=VECTOR('',#4187,1.);
#1276=VECTOR('',#4188,1.);
#1277=VECTOR('',#4189,1.);
#1278=VECTOR('',#4192,1.);
#1279=VECTOR('',#4193,1.);
#1280=VECTOR('',#4194,1.);
#1281=VECTOR('',#4197,1.);
#1282=VECTOR('',#4198,1.);
#1283=VECTOR('',#4199,1.);
#1284=VECTOR('',#4202,1.);
#1285=VECTOR('',#4203,1.);
#1286=VECTOR('',#4214,0.205);
#1287=VECTOR('',#4221,0.33);
#1288=VECTOR('',#4228,0.33);
#1289=VECTOR('',#4235,0.625);
#1290=VECTOR('',#4246,0.625);
#1291=VECTOR('',#4255,0.33);
#1292=VECTOR('',#4260,0.33);
#1293=VECTOR('',#4265,1.);
#1294=VECTOR('',#4266,1.);
#1295=VECTOR('',#4267,1.);
#1296=VECTOR('',#4268,1.);
#1297=VECTOR('',#4271,1.);
#1298=VECTOR('',#4272,1.);
#1299=VECTOR('',#4273,1.);
#1300=VECTOR('',#4276,1.);
#1301=VECTOR('',#4277,1.);
#1302=VECTOR('',#4278,1.);
#1303=VECTOR('',#4281,1.);
#1304=VECTOR('',#4282,1.);
#1305=VECTOR('',#4299,0.46);
#1306=VECTOR('',#4302,1.);
#1307=VECTOR('',#4303,1.);
#1308=VECTOR('',#4304,1.);
#1309=VECTOR('',#4305,1.);
#1310=VECTOR('',#4306,1.);
#1311=VECTOR('',#4307,1.);
#1312=VECTOR('',#4312,1.);
#1313=VECTOR('',#4313,1.);
#1314=VECTOR('',#4314,1.);
#1315=VECTOR('',#4315,1.);
#1316=VECTOR('',#4316,1.);
#1317=VECTOR('',#4317,1.);
#1318=VECTOR('',#4322,1.);
#1319=VECTOR('',#4323,1.);
#1320=VECTOR('',#4326,1.);
#1321=VECTOR('',#4329,1.);
#1322=VECTOR('',#4332,1.);
#1323=VECTOR('',#4335,1.);
#1324=VECTOR('',#4340,0.685);
#1325=VECTOR('',#4345,0.685);
#1326=VECTOR('',#4350,0.645);
#1327=VECTOR('',#4359,0.685);
#1328=VECTOR('',#4366,1.);
#1329=VECTOR('',#4367,1.);
#1330=VECTOR('',#4368,1.);
#1331=VECTOR('',#4369,1.);
#1332=VECTOR('',#4370,1.);
#1333=VECTOR('',#4371,1.);
#1334=VECTOR('',#4374,1.);
#1335=VECTOR('',#4375,1.);
#1336=VECTOR('',#4376,1.);
#1337=VECTOR('',#4379,1.);
#1338=VECTOR('',#4380,1.);
#1339=VECTOR('',#4383,1.);
#1340=VECTOR('',#4384,1.);
#1341=VECTOR('',#4387,1.);
#1342=VECTOR('',#4388,1.);
#1343=VECTOR('',#4391,1.);
#1344=VECTOR('',#4392,1.);
#1345=VECTOR('',#4395,1.);
#1346=VECTOR('',#4406,0.43);
#1347=VECTOR('',#4415,1.);
#1348=VECTOR('',#4416,1.);
#1349=VECTOR('',#4417,1.);
#1350=VECTOR('',#4418,1.);
#1351=VECTOR('',#4419,1.);
#1352=VECTOR('',#4420,1.);
#1353=VECTOR('',#4425,1.);
#1354=VECTOR('',#4426,1.);
#1355=VECTOR('',#4427,1.);
#1356=VECTOR('',#4428,1.);
#1357=VECTOR('',#4429,1.);
#1358=VECTOR('',#4430,1.);
#1359=VECTOR('',#4435,1.);
#1360=VECTOR('',#4436,1.);
#1361=VECTOR('',#4439,1.);
#1362=VECTOR('',#4442,1.);
#1363=VECTOR('',#4445,1.);
#1364=VECTOR('',#4448,1.);
#1365=VECTOR('',#4457,0.46);
#1366=VECTOR('',#4466,0.525);
#1367=VECTOR('',#4471,0.515);
#1368=VECTOR('',#4478,0.2);
#1369=VECTOR('',#4491,0.475);
#1370=VECTOR('',#4500,0.355);
#1371=VECTOR('',#4507,0.31);
#1372=VECTOR('',#4522,0.2);
#1373=VECTOR('',#4527,0.17);
#1374=VECTOR('',#4536,0.32);
#1375=VECTOR('',#4543,0.6);
#1376=VECTOR('',#4556,0.3);
#1377=VECTOR('',#4563,0.27);
#1378=VECTOR('',#4570,0.576175134594813);
#1379=VECTOR('',#4573,1.);
#1380=VECTOR('',#4574,1.);
#1381=VECTOR('',#4575,1.);
#1382=VECTOR('',#4578,1.);
#1383=VECTOR('',#4579,1.);
#1384=VECTOR('',#4582,1.);
#1385=VECTOR('',#4583,1.);
#1386=VECTOR('',#4586,1.);
#1387=VECTOR('',#4587,1.);
#1388=VECTOR('',#4590,1.);
#1389=VECTOR('',#4591,1.);
#1390=VECTOR('',#4594,1.);
#1391=VERTEX_POINT('',#4648);
#1392=VERTEX_POINT('',#4649);
#1393=VERTEX_POINT('',#4653);
#1394=VERTEX_POINT('',#4654);
#1395=VERTEX_POINT('',#4657);
#1396=VERTEX_POINT('',#4659);
#1397=VERTEX_POINT('',#4662);
#1398=VERTEX_POINT('',#4666);
#1399=VERTEX_POINT('',#4667);
#1400=VERTEX_POINT('',#4671);
#1401=VERTEX_POINT('',#4672);
#1402=VERTEX_POINT('',#4676);
#1403=VERTEX_POINT('',#4677);
#1404=VERTEX_POINT('',#4679);
#1405=VERTEX_POINT('',#4682);
#1406=VERTEX_POINT('',#4684);
#1407=VERTEX_POINT('',#4686);
#1408=VERTEX_POINT('',#4688);
#1409=VERTEX_POINT('',#4692);
#1410=VERTEX_POINT('',#4694);
#1411=VERTEX_POINT('',#4696);
#1412=VERTEX_POINT('',#4734);
#1413=VERTEX_POINT('',#4736);
#1414=VERTEX_POINT('',#4741);
#1415=VERTEX_POINT('',#4743);
#1416=VERTEX_POINT('',#4748);
#1417=VERTEX_POINT('',#4750);
#1418=VERTEX_POINT('',#4755);
#1419=VERTEX_POINT('',#4757);
#1420=VERTEX_POINT('',#4762);
#1421=VERTEX_POINT('',#4764);
#1422=VERTEX_POINT('',#4766);
#1423=VERTEX_POINT('',#4804);
#1424=VERTEX_POINT('',#4806);
#1425=VERTEX_POINT('',#4811);
#1426=VERTEX_POINT('',#4813);
#1427=VERTEX_POINT('',#4818);
#1428=VERTEX_POINT('',#4820);
#1429=VERTEX_POINT('',#4825);
#1430=VERTEX_POINT('',#4827);
#1431=VERTEX_POINT('',#4834);
#1432=VERTEX_POINT('',#4838);
#1433=VERTEX_POINT('',#4840);
#1434=VERTEX_POINT('',#4842);
#1435=VERTEX_POINT('',#4844);
#1436=VERTEX_POINT('',#4846);
#1437=VERTEX_POINT('',#4848);
#1438=VERTEX_POINT('',#4850);
#1439=VERTEX_POINT('',#4852);
#1440=VERTEX_POINT('',#4855);
#1441=VERTEX_POINT('',#4866);
#1442=VERTEX_POINT('',#4872);
#1443=VERTEX_POINT('',#4878);
#1444=VERTEX_POINT('',#4879);
#1445=VERTEX_POINT('',#4881);
#1446=VERTEX_POINT('',#4883);
#1447=VERTEX_POINT('',#4887);
#1448=VERTEX_POINT('',#4889);
#1449=VERTEX_POINT('',#4893);
#1450=VERTEX_POINT('',#4895);
#1451=VERTEX_POINT('',#4905);
#1452=VERTEX_POINT('',#4907);
#1453=VERTEX_POINT('',#4911);
#1454=VERTEX_POINT('',#4914);
#1455=VERTEX_POINT('',#4915);
#1456=VERTEX_POINT('',#4917);
#1457=VERTEX_POINT('',#4919);
#1458=VERTEX_POINT('',#4921);
#1459=VERTEX_POINT('',#4923);
#1460=VERTEX_POINT('',#4926);
#1461=VERTEX_POINT('',#4929);
#1462=VERTEX_POINT('',#4931);
#1463=VERTEX_POINT('',#4935);
#1464=VERTEX_POINT('',#4939);
#1465=VERTEX_POINT('',#4943);
#1466=VERTEX_POINT('',#4947);
#1467=VERTEX_POINT('',#4954);
#1468=VERTEX_POINT('',#4958);
#1469=VERTEX_POINT('',#4964);
#1470=VERTEX_POINT('',#4966);
#1471=VERTEX_POINT('',#4970);
#1472=VERTEX_POINT('',#4973);
#1473=VERTEX_POINT('',#4974);
#1474=VERTEX_POINT('',#4976);
#1475=VERTEX_POINT('',#4978);
#1476=VERTEX_POINT('',#4980);
#1477=VERTEX_POINT('',#4982);
#1478=VERTEX_POINT('',#4985);
#1479=VERTEX_POINT('',#4988);
#1480=VERTEX_POINT('',#4990);
#1481=VERTEX_POINT('',#4994);
#1482=VERTEX_POINT('',#4998);
#1483=VERTEX_POINT('',#5002);
#1484=VERTEX_POINT('',#5006);
#1485=VERTEX_POINT('',#5013);
#1486=VERTEX_POINT('',#5017);
#1487=VERTEX_POINT('',#5023);
#1488=VERTEX_POINT('',#5025);
#1489=VERTEX_POINT('',#5029);
#1490=VERTEX_POINT('',#5032);
#1491=VERTEX_POINT('',#5033);
#1492=VERTEX_POINT('',#5035);
#1493=VERTEX_POINT('',#5037);
#1494=VERTEX_POINT('',#5039);
#1495=VERTEX_POINT('',#5041);
#1496=VERTEX_POINT('',#5044);
#1497=VERTEX_POINT('',#5047);
#1498=VERTEX_POINT('',#5049);
#1499=VERTEX_POINT('',#5053);
#1500=VERTEX_POINT('',#5057);
#1501=VERTEX_POINT('',#5061);
#1502=VERTEX_POINT('',#5065);
#1503=VERTEX_POINT('',#5072);
#1504=VERTEX_POINT('',#5076);
#1505=VERTEX_POINT('',#5082);
#1506=VERTEX_POINT('',#5084);
#1507=VERTEX_POINT('',#5088);
#1508=VERTEX_POINT('',#5091);
#1509=VERTEX_POINT('',#5092);
#1510=VERTEX_POINT('',#5094);
#1511=VERTEX_POINT('',#5096);
#1512=VERTEX_POINT('',#5098);
#1513=VERTEX_POINT('',#5100);
#1514=VERTEX_POINT('',#5103);
#1515=VERTEX_POINT('',#5106);
#1516=VERTEX_POINT('',#5108);
#1517=VERTEX_POINT('',#5112);
#1518=VERTEX_POINT('',#5116);
#1519=VERTEX_POINT('',#5120);
#1520=VERTEX_POINT('',#5124);
#1521=VERTEX_POINT('',#5131);
#1522=VERTEX_POINT('',#5135);
#1523=VERTEX_POINT('',#5141);
#1524=VERTEX_POINT('',#5143);
#1525=VERTEX_POINT('',#5147);
#1526=VERTEX_POINT('',#5149);
#1527=VERTEX_POINT('',#5153);
#1528=VERTEX_POINT('',#5155);
#1529=VERTEX_POINT('',#5159);
#1530=VERTEX_POINT('',#5161);
#1531=VERTEX_POINT('',#5165);
#1532=VERTEX_POINT('',#5168);
#1533=VERTEX_POINT('',#5170);
#1534=VERTEX_POINT('',#5174);
#1535=VERTEX_POINT('',#5177);
#1536=VERTEX_POINT('',#5181);
#1537=VERTEX_POINT('',#5185);
#1538=VERTEX_POINT('',#5186);
#1539=VERTEX_POINT('',#5188);
#1540=VERTEX_POINT('',#5190);
#1541=VERTEX_POINT('',#5194);
#1542=VERTEX_POINT('',#5196);
#1543=VERTEX_POINT('',#5200);
#1544=VERTEX_POINT('',#5202);
#1545=VERTEX_POINT('',#5212);
#1546=VERTEX_POINT('',#5214);
#1547=VERTEX_POINT('',#5218);
#1548=VERTEX_POINT('',#5220);
#1549=VERTEX_POINT('',#5224);
#1550=VERTEX_POINT('',#5226);
#1551=VERTEX_POINT('',#5230);
#1552=VERTEX_POINT('',#5232);
#1553=VERTEX_POINT('',#5236);
#1554=VERTEX_POINT('',#5239);
#1555=VERTEX_POINT('',#5241);
#1556=VERTEX_POINT('',#5245);
#1557=VERTEX_POINT('',#5248);
#1558=VERTEX_POINT('',#5252);
#1559=VERTEX_POINT('',#5256);
#1560=VERTEX_POINT('',#5257);
#1561=VERTEX_POINT('',#5259);
#1562=VERTEX_POINT('',#5261);
#1563=VERTEX_POINT('',#5265);
#1564=VERTEX_POINT('',#5267);
#1565=VERTEX_POINT('',#5271);
#1566=VERTEX_POINT('',#5273);
#1567=VERTEX_POINT('',#5283);
#1568=VERTEX_POINT('',#5285);
#1569=VERTEX_POINT('',#5288);
#1570=VERTEX_POINT('',#5292);
#1571=VERTEX_POINT('',#5293);
#1572=VERTEX_POINT('',#5295);
#1573=VERTEX_POINT('',#5297);
#1574=VERTEX_POINT('',#5299);
#1575=VERTEX_POINT('',#5301);
#1576=VERTEX_POINT('',#5304);
#1577=VERTEX_POINT('',#5307);
#1578=VERTEX_POINT('',#5308);
#1579=VERTEX_POINT('',#5310);
#1580=VERTEX_POINT('',#5312);
#1581=VERTEX_POINT('',#5314);
#1582=VERTEX_POINT('',#5316);
#1583=VERTEX_POINT('',#5319);
#1584=VERTEX_POINT('',#5336);
#1585=VERTEX_POINT('',#5340);
#1586=VERTEX_POINT('',#5346);
#1587=VERTEX_POINT('',#5348);
#1588=VERTEX_POINT('',#5353);
#1589=VERTEX_POINT('',#5354);
#1590=VERTEX_POINT('',#5356);
#1591=VERTEX_POINT('',#5358);
#1592=VERTEX_POINT('',#5360);
#1593=VERTEX_POINT('',#5362);
#1594=VERTEX_POINT('',#5366);
#1595=VERTEX_POINT('',#5368);
#1596=VERTEX_POINT('',#5372);
#1597=VERTEX_POINT('',#5376);
#1598=VERTEX_POINT('',#5380);
#1599=VERTEX_POINT('',#5384);
#1600=VERTEX_POINT('',#5393);
#1601=VERTEX_POINT('',#5395);
#1602=VERTEX_POINT('',#5399);
#1603=VERTEX_POINT('',#5402);
#1604=VERTEX_POINT('',#5403);
#1605=VERTEX_POINT('',#5405);
#1606=VERTEX_POINT('',#5407);
#1607=VERTEX_POINT('',#5409);
#1608=VERTEX_POINT('',#5411);
#1609=VERTEX_POINT('',#5414);
#1610=VERTEX_POINT('',#5417);
#1611=VERTEX_POINT('',#5418);
#1612=VERTEX_POINT('',#5420);
#1613=VERTEX_POINT('',#5422);
#1614=VERTEX_POINT('',#5424);
#1615=VERTEX_POINT('',#5426);
#1616=VERTEX_POINT('',#5429);
#1617=VERTEX_POINT('',#5444);
#1618=VERTEX_POINT('',#5447);
#1619=VERTEX_POINT('',#5451);
#1620=VERTEX_POINT('',#5456);
#1621=VERTEX_POINT('',#5460);
#1622=VERTEX_POINT('',#5466);
#1623=VERTEX_POINT('',#5468);
#1624=VERTEX_POINT('',#5471);
#1625=VERTEX_POINT('',#5475);
#1626=VERTEX_POINT('',#5478);
#1627=VERTEX_POINT('',#5482);
#1628=VERTEX_POINT('',#5490);
#1629=VERTEX_POINT('',#5493);
#1630=VERTEX_POINT('',#5497);
#1631=VERTEX_POINT('',#5503);
#1632=VERTEX_POINT('',#5505);
#1633=VERTEX_POINT('',#5509);
#1634=VERTEX_POINT('',#5511);
#1635=VERTEX_POINT('',#5518);
#1636=VERTEX_POINT('',#5520);
#1637=VERTEX_POINT('',#5524);
#1638=VERTEX_POINT('',#5529);
#1639=VERTEX_POINT('',#5531);
#1640=VERTEX_POINT('',#5533);
#1641=VERTEX_POINT('',#5537);
#1642=VERTEX_POINT('',#5541);
#1643=VERTEX_POINT('',#5545);
#1644=VERTEX_POINT('',#5549);
#1645=VERTEX_POINT('',#5557);
#1646=VERTEX_POINT('',#5559);
#1647=VERTEX_POINT('',#5563);
#1648=VERTEX_POINT('',#5567);
#1649=VERTEX_POINT('',#5571);
#1650=VERTEX_POINT('',#5575);
#1651=EDGE_CURVE('',#1391,#1392,#897,.T.);
#1652=EDGE_CURVE('',#1392,#1391,#777,.T.);
#1653=EDGE_CURVE('',#1393,#1394,#257,.T.);
#1654=EDGE_CURVE('',#1394,#1391,#258,.T.);
#1655=EDGE_CURVE('',#1392,#1395,#259,.T.);
#1656=EDGE_CURVE('',#1395,#1396,#898,.T.);
#1657=EDGE_CURVE('',#1396,#1396,#778,.T.);
#1658=EDGE_CURVE('',#1395,#1397,#260,.T.);
#1659=EDGE_CURVE('',#1393,#1397,#779,.T.);
#1660=EDGE_CURVE('',#1398,#1399,#899,.T.);
#1661=EDGE_CURVE('',#1399,#1398,#780,.T.);
#1662=EDGE_CURVE('',#1400,#1401,#900,.T.);
#1663=EDGE_CURVE('',#1401,#1400,#781,.T.);
#1664=EDGE_CURVE('',#1402,#1403,#261,.T.);
#1665=EDGE_CURVE('',#1403,#1404,#901,.T.);
#1666=EDGE_CURVE('',#1404,#1404,#782,.T.);
#1667=EDGE_CURVE('',#1403,#1405,#262,.T.);
#1668=EDGE_CURVE('',#1406,#1405,#783,.T.);
#1669=EDGE_CURVE('',#1406,#1407,#263,.T.);
#1670=EDGE_CURVE('',#1407,#1408,#264,.T.);
#1671=EDGE_CURVE('',#1402,#1408,#784,.T.);
#1672=EDGE_CURVE('',#1409,#1409,#785,.T.);
#1673=EDGE_CURVE('',#1409,#1410,#902,.T.);
#1674=EDGE_CURVE('',#1411,#1410,#253,.T.);
#1675=EDGE_CURVE('',#1410,#1411,#254,.T.);
#1676=EDGE_CURVE('',#1412,#1412,#786,.T.);
#1677=EDGE_CURVE('',#1412,#1413,#903,.T.);
#1678=EDGE_CURVE('',#1413,#1413,#787,.T.);
#1679=EDGE_CURVE('',#1414,#1414,#788,.T.);
#1680=EDGE_CURVE('',#1414,#1415,#904,.T.);
#1681=EDGE_CURVE('',#1415,#1415,#789,.T.);
#1682=EDGE_CURVE('',#1416,#1416,#790,.T.);
#1683=EDGE_CURVE('',#1416,#1417,#905,.T.);
#1684=EDGE_CURVE('',#1417,#1417,#791,.T.);
#1685=EDGE_CURVE('',#1418,#1418,#792,.T.);
#1686=EDGE_CURVE('',#1418,#1419,#906,.T.);
#1687=EDGE_CURVE('',#1419,#1419,#793,.T.);
#1688=EDGE_CURVE('',#1420,#1420,#794,.T.);
#1689=EDGE_CURVE('',#1420,#1421,#907,.T.);
#1690=EDGE_CURVE('',#1422,#1421,#255,.T.);
#1691=EDGE_CURVE('',#1421,#1422,#256,.T.);
#1692=EDGE_CURVE('',#1423,#1423,#795,.T.);
#1693=EDGE_CURVE('',#1423,#1424,#908,.T.);
#1694=EDGE_CURVE('',#1424,#1424,#796,.T.);
#1695=EDGE_CURVE('',#1425,#1425,#797,.T.);
#1696=EDGE_CURVE('',#1425,#1426,#909,.T.);
#1697=EDGE_CURVE('',#1426,#1426,#798,.T.);
#1698=EDGE_CURVE('',#1427,#1427,#799,.T.);
#1699=EDGE_CURVE('',#1427,#1428,#910,.T.);
#1700=EDGE_CURVE('',#1428,#1428,#800,.T.);
#1701=EDGE_CURVE('',#1429,#1429,#801,.T.);
#1702=EDGE_CURVE('',#1429,#1430,#911,.T.);
#1703=EDGE_CURVE('',#1430,#1430,#802,.T.);
#1704=EDGE_CURVE('',#1397,#1393,#912,.T.);
#1705=EDGE_CURVE('',#1431,#1431,#803,.T.);
#1706=EDGE_CURVE('',#1431,#1403,#913,.T.);
#1707=EDGE_CURVE('',#1408,#1402,#914,.T.);
#1708=EDGE_CURVE('',#1407,#1432,#915,.T.);
#1709=EDGE_CURVE('',#1433,#1432,#265,.T.);
#1710=EDGE_CURVE('',#1434,#1433,#916,.T.);
#1711=EDGE_CURVE('',#1435,#1434,#266,.T.);
#1712=EDGE_CURVE('',#1435,#1436,#917,.T.);
#1713=EDGE_CURVE('',#1437,#1436,#267,.T.);
#1714=EDGE_CURVE('',#1438,#1437,#918,.T.);
#1715=EDGE_CURVE('',#1439,#1438,#268,.T.);
#1716=EDGE_CURVE('',#1439,#1395,#919,.T.);
#1717=EDGE_CURVE('',#1394,#1440,#920,.T.);
#1718=EDGE_CURVE('',#1440,#1440,#804,.T.);
#1719=EDGE_CURVE('',#1399,#1439,#269,.T.);
#1720=EDGE_CURVE('',#1436,#1398,#270,.T.);
#1721=EDGE_CURVE('',#1401,#1435,#271,.T.);
#1722=EDGE_CURVE('',#1432,#1400,#272,.T.);
#1723=EDGE_CURVE('',#1405,#1406,#921,.T.);
#1724=EDGE_CURVE('',#1437,#1438,#805,.T.);
#1725=EDGE_CURVE('',#1436,#1441,#922,.T.);
#1726=EDGE_CURVE('',#1441,#1441,#806,.T.);
#1727=EDGE_CURVE('',#1433,#1434,#807,.T.);
#1728=EDGE_CURVE('',#1432,#1442,#923,.T.);
#1729=EDGE_CURVE('',#1442,#1442,#808,.T.);
#1730=EDGE_CURVE('',#1443,#1444,#924,.T.);
#1731=EDGE_CURVE('',#1444,#1445,#925,.T.);
#1732=EDGE_CURVE('',#1446,#1445,#926,.T.);
#1733=EDGE_CURVE('',#1443,#1446,#927,.T.);
#1734=EDGE_CURVE('',#1447,#1443,#928,.T.);
#1735=EDGE_CURVE('',#1448,#1446,#929,.T.);
#1736=EDGE_CURVE('',#1447,#1448,#930,.T.);
#1737=EDGE_CURVE('',#1449,#1447,#931,.T.);
#1738=EDGE_CURVE('',#1450,#1448,#932,.T.);
#1739=EDGE_CURVE('',#1449,#1450,#933,.T.);
#1740=EDGE_CURVE('',#1444,#1449,#934,.T.);
#1741=EDGE_CURVE('',#1445,#1450,#935,.T.);
#1742=EDGE_CURVE('',#1451,#1451,#809,.T.);
#1743=EDGE_CURVE('',#1451,#1452,#936,.T.);
#1744=EDGE_CURVE('',#1452,#1452,#810,.T.);
#1745=EDGE_CURVE('',#1453,#1453,#811,.T.);
#1746=EDGE_CURVE('',#1454,#1455,#937,.T.);
#1747=EDGE_CURVE('',#1456,#1454,#938,.T.);
#1748=EDGE_CURVE('',#1457,#1456,#939,.T.);
#1749=EDGE_CURVE('',#1458,#1457,#940,.T.);
#1750=EDGE_CURVE('',#1459,#1458,#941,.T.);
#1751=EDGE_CURVE('',#1455,#1459,#942,.T.);
#1752=EDGE_CURVE('',#1460,#1460,#812,.T.);
#1753=EDGE_CURVE('',#1454,#1461,#943,.T.);
#1754=EDGE_CURVE('',#1462,#1461,#944,.T.);
#1755=EDGE_CURVE('',#1456,#1462,#945,.T.);
#1756=EDGE_CURVE('',#1463,#1462,#946,.T.);
#1757=EDGE_CURVE('',#1457,#1463,#947,.T.);
#1758=EDGE_CURVE('',#1464,#1463,#948,.T.);
#1759=EDGE_CURVE('',#1458,#1464,#949,.T.);
#1760=EDGE_CURVE('',#1465,#1464,#950,.T.);
#1761=EDGE_CURVE('',#1459,#1465,#951,.T.);
#1762=EDGE_CURVE('',#1466,#1465,#952,.T.);
#1763=EDGE_CURVE('',#1455,#1466,#953,.T.);
#1764=EDGE_CURVE('',#1461,#1466,#954,.T.);
#1765=EDGE_CURVE('',#1453,#1467,#955,.T.);
#1766=EDGE_CURVE('',#1467,#1467,#813,.T.);
#1767=EDGE_CURVE('',#1460,#1468,#956,.T.);
#1768=EDGE_CURVE('',#1468,#1468,#814,.T.);
#1769=EDGE_CURVE('',#1469,#1469,#815,.T.);
#1770=EDGE_CURVE('',#1469,#1470,#957,.T.);
#1771=EDGE_CURVE('',#1470,#1470,#816,.T.);
#1772=EDGE_CURVE('',#1471,#1471,#817,.T.);
#1773=EDGE_CURVE('',#1472,#1473,#958,.T.);
#1774=EDGE_CURVE('',#1474,#1472,#959,.T.);
#1775=EDGE_CURVE('',#1475,#1474,#960,.T.);
#1776=EDGE_CURVE('',#1476,#1475,#961,.T.);
#1777=EDGE_CURVE('',#1477,#1476,#962,.T.);
#1778=EDGE_CURVE('',#1473,#1477,#963,.T.);
#1779=EDGE_CURVE('',#1478,#1478,#818,.T.);
#1780=EDGE_CURVE('',#1472,#1479,#964,.T.);
#1781=EDGE_CURVE('',#1480,#1479,#965,.T.);
#1782=EDGE_CURVE('',#1474,#1480,#966,.T.);
#1783=EDGE_CURVE('',#1481,#1480,#967,.T.);
#1784=EDGE_CURVE('',#1475,#1481,#968,.T.);
#1785=EDGE_CURVE('',#1482,#1481,#969,.T.);
#1786=EDGE_CURVE('',#1476,#1482,#970,.T.);
#1787=EDGE_CURVE('',#1483,#1482,#971,.T.);
#1788=EDGE_CURVE('',#1477,#1483,#972,.T.);
#1789=EDGE_CURVE('',#1484,#1483,#973,.T.);
#1790=EDGE_CURVE('',#1473,#1484,#974,.T.);
#1791=EDGE_CURVE('',#1479,#1484,#975,.T.);
#1792=EDGE_CURVE('',#1471,#1485,#976,.T.);
#1793=EDGE_CURVE('',#1485,#1485,#819,.T.);
#1794=EDGE_CURVE('',#1478,#1486,#977,.T.);
#1795=EDGE_CURVE('',#1486,#1486,#820,.T.);
#1796=EDGE_CURVE('',#1487,#1487,#821,.T.);
#1797=EDGE_CURVE('',#1487,#1488,#978,.T.);
#1798=EDGE_CURVE('',#1488,#1488,#822,.T.);
#1799=EDGE_CURVE('',#1489,#1489,#823,.T.);
#1800=EDGE_CURVE('',#1490,#1491,#979,.T.);
#1801=EDGE_CURVE('',#1492,#1490,#980,.T.);
#1802=EDGE_CURVE('',#1493,#1492,#981,.T.);
#1803=EDGE_CURVE('',#1494,#1493,#982,.T.);
#1804=EDGE_CURVE('',#1495,#1494,#983,.T.);
#1805=EDGE_CURVE('',#1491,#1495,#984,.T.);
#1806=EDGE_CURVE('',#1496,#1496,#824,.T.);
#1807=EDGE_CURVE('',#1490,#1497,#985,.T.);
#1808=EDGE_CURVE('',#1498,#1497,#986,.T.);
#1809=EDGE_CURVE('',#1492,#1498,#987,.T.);
#1810=EDGE_CURVE('',#1499,#1498,#988,.T.);
#1811=EDGE_CURVE('',#1493,#1499,#989,.T.);
#1812=EDGE_CURVE('',#1500,#1499,#990,.T.);
#1813=EDGE_CURVE('',#1494,#1500,#991,.T.);
#1814=EDGE_CURVE('',#1501,#1500,#992,.T.);
#1815=EDGE_CURVE('',#1495,#1501,#993,.T.);
#1816=EDGE_CURVE('',#1502,#1501,#994,.T.);
#1817=EDGE_CURVE('',#1491,#1502,#995,.T.);
#1818=EDGE_CURVE('',#1497,#1502,#996,.T.);
#1819=EDGE_CURVE('',#1489,#1503,#997,.T.);
#1820=EDGE_CURVE('',#1503,#1503,#825,.T.);
#1821=EDGE_CURVE('',#1496,#1504,#998,.T.);
#1822=EDGE_CURVE('',#1504,#1504,#826,.T.);
#1823=EDGE_CURVE('',#1505,#1505,#827,.T.);
#1824=EDGE_CURVE('',#1505,#1506,#999,.T.);
#1825=EDGE_CURVE('',#1506,#1506,#828,.T.);
#1826=EDGE_CURVE('',#1507,#1507,#829,.T.);
#1827=EDGE_CURVE('',#1508,#1509,#1000,.T.);
#1828=EDGE_CURVE('',#1510,#1508,#1001,.T.);
#1829=EDGE_CURVE('',#1511,#1510,#1002,.T.);
#1830=EDGE_CURVE('',#1512,#1511,#1003,.T.);
#1831=EDGE_CURVE('',#1513,#1512,#1004,.T.);
#1832=EDGE_CURVE('',#1509,#1513,#1005,.T.);
#1833=EDGE_CURVE('',#1514,#1514,#830,.T.);
#1834=EDGE_CURVE('',#1508,#1515,#1006,.T.);
#1835=EDGE_CURVE('',#1516,#1515,#1007,.T.);
#1836=EDGE_CURVE('',#1510,#1516,#1008,.T.);
#1837=EDGE_CURVE('',#1517,#1516,#1009,.T.);
#1838=EDGE_CURVE('',#1511,#1517,#1010,.T.);
#1839=EDGE_CURVE('',#1518,#1517,#1011,.T.);
#1840=EDGE_CURVE('',#1512,#1518,#1012,.T.);
#1841=EDGE_CURVE('',#1519,#1518,#1013,.T.);
#1842=EDGE_CURVE('',#1513,#1519,#1014,.T.);
#1843=EDGE_CURVE('',#1520,#1519,#1015,.T.);
#1844=EDGE_CURVE('',#1509,#1520,#1016,.T.);
#1845=EDGE_CURVE('',#1515,#1520,#1017,.T.);
#1846=EDGE_CURVE('',#1507,#1521,#1018,.T.);
#1847=EDGE_CURVE('',#1521,#1521,#831,.T.);
#1848=EDGE_CURVE('',#1514,#1522,#1019,.T.);
#1849=EDGE_CURVE('',#1522,#1522,#832,.T.);
#1850=EDGE_CURVE('',#1523,#1523,#833,.T.);
#1851=EDGE_CURVE('',#1523,#1524,#1020,.T.);
#1852=EDGE_CURVE('',#1524,#1524,#834,.T.);
#1853=EDGE_CURVE('',#1525,#1525,#835,.T.);
#1854=EDGE_CURVE('',#1525,#1526,#1021,.T.);
#1855=EDGE_CURVE('',#1526,#1526,#836,.T.);
#1856=EDGE_CURVE('',#1527,#1527,#837,.T.);
#1857=EDGE_CURVE('',#1527,#1528,#1022,.T.);
#1858=EDGE_CURVE('',#1528,#1528,#838,.T.);
#1859=EDGE_CURVE('',#1529,#1529,#839,.T.);
#1860=EDGE_CURVE('',#1529,#1530,#1023,.T.);
#1861=EDGE_CURVE('',#1530,#1530,#840,.T.);
#1862=EDGE_CURVE('',#1531,#1531,#841,.T.);
#1863=EDGE_CURVE('',#1532,#1532,#842,.T.);
#1864=EDGE_CURVE('',#1532,#1533,#1024,.T.);
#1865=EDGE_CURVE('',#1533,#1533,#843,.T.);
#1866=EDGE_CURVE('',#1534,#1534,#844,.T.);
#1867=EDGE_CURVE('',#1531,#1535,#1025,.T.);
#1868=EDGE_CURVE('',#1535,#1535,#845,.T.);
#1869=EDGE_CURVE('',#1534,#1536,#1026,.T.);
#1870=EDGE_CURVE('',#1536,#1536,#846,.T.);
#1871=EDGE_CURVE('',#1537,#1538,#1027,.T.);
#1872=EDGE_CURVE('',#1538,#1539,#1028,.T.);
#1873=EDGE_CURVE('',#1540,#1539,#1029,.T.);
#1874=EDGE_CURVE('',#1537,#1540,#1030,.T.);
#1875=EDGE_CURVE('',#1541,#1537,#1031,.T.);
#1876=EDGE_CURVE('',#1542,#1540,#1032,.T.);
#1877=EDGE_CURVE('',#1541,#1542,#1033,.T.);
#1878=EDGE_CURVE('',#1543,#1541,#1034,.T.);
#1879=EDGE_CURVE('',#1544,#1542,#1035,.T.);
#1880=EDGE_CURVE('',#1543,#1544,#1036,.T.);
#1881=EDGE_CURVE('',#1538,#1543,#1037,.T.);
#1882=EDGE_CURVE('',#1539,#1544,#1038,.T.);
#1883=EDGE_CURVE('',#1545,#1545,#847,.T.);
#1884=EDGE_CURVE('',#1545,#1546,#1039,.T.);
#1885=EDGE_CURVE('',#1546,#1546,#848,.T.);
#1886=EDGE_CURVE('',#1547,#1547,#849,.T.);
#1887=EDGE_CURVE('',#1547,#1548,#1040,.T.);
#1888=EDGE_CURVE('',#1548,#1548,#850,.T.);
#1889=EDGE_CURVE('',#1549,#1549,#851,.T.);
#1890=EDGE_CURVE('',#1549,#1550,#1041,.T.);
#1891=EDGE_CURVE('',#1550,#1550,#852,.T.);
#1892=EDGE_CURVE('',#1551,#1551,#853,.T.);
#1893=EDGE_CURVE('',#1551,#1552,#1042,.T.);
#1894=EDGE_CURVE('',#1552,#1552,#854,.T.);
#1895=EDGE_CURVE('',#1553,#1553,#855,.T.);
#1896=EDGE_CURVE('',#1554,#1554,#856,.T.);
#1897=EDGE_CURVE('',#1554,#1555,#1043,.T.);
#1898=EDGE_CURVE('',#1555,#1555,#857,.T.);
#1899=EDGE_CURVE('',#1556,#1556,#858,.T.);
#1900=EDGE_CURVE('',#1553,#1557,#1044,.T.);
#1901=EDGE_CURVE('',#1557,#1557,#859,.T.);
#1902=EDGE_CURVE('',#1556,#1558,#1045,.T.);
#1903=EDGE_CURVE('',#1558,#1558,#860,.T.);
#1904=EDGE_CURVE('',#1559,#1560,#1046,.T.);
#1905=EDGE_CURVE('',#1560,#1561,#1047,.T.);
#1906=EDGE_CURVE('',#1562,#1561,#1048,.T.);
#1907=EDGE_CURVE('',#1559,#1562,#1049,.T.);
#1908=EDGE_CURVE('',#1563,#1559,#1050,.T.);
#1909=EDGE_CURVE('',#1564,#1562,#1051,.T.);
#1910=EDGE_CURVE('',#1563,#1564,#1052,.T.);
#1911=EDGE_CURVE('',#1565,#1563,#1053,.T.);
#1912=EDGE_CURVE('',#1566,#1564,#1054,.T.);
#1913=EDGE_CURVE('',#1565,#1566,#1055,.T.);
#1914=EDGE_CURVE('',#1560,#1565,#1056,.T.);
#1915=EDGE_CURVE('',#1561,#1566,#1057,.T.);
#1916=EDGE_CURVE('',#1567,#1567,#861,.T.);
#1917=EDGE_CURVE('',#1568,#1568,#862,.T.);
#1918=EDGE_CURVE('',#1569,#1569,#863,.T.);
#1919=EDGE_CURVE('',#1569,#1568,#1058,.T.);
#1920=EDGE_CURVE('',#1570,#1571,#1059,.T.);
#1921=EDGE_CURVE('',#1571,#1572,#1060,.T.);
#1922=EDGE_CURVE('',#1572,#1573,#1061,.T.);
#1923=EDGE_CURVE('',#1573,#1574,#1062,.T.);
#1924=EDGE_CURVE('',#1574,#1575,#1063,.T.);
#1925=EDGE_CURVE('',#1575,#1570,#1064,.T.);
#1926=EDGE_CURVE('',#1576,#1576,#864,.T.);
#1927=EDGE_CURVE('',#1577,#1578,#1065,.T.);
#1928=EDGE_CURVE('',#1578,#1579,#1066,.T.);
#1929=EDGE_CURVE('',#1579,#1580,#1067,.T.);
#1930=EDGE_CURVE('',#1580,#1581,#1068,.T.);
#1931=EDGE_CURVE('',#1581,#1582,#1069,.T.);
#1932=EDGE_CURVE('',#1582,#1577,#1070,.T.);
#1933=EDGE_CURVE('',#1583,#1583,#865,.T.);
#1934=EDGE_CURVE('',#1577,#1571,#1071,.T.);
#1935=EDGE_CURVE('',#1572,#1582,#1072,.T.);
#1936=EDGE_CURVE('',#1573,#1581,#1073,.T.);
#1937=EDGE_CURVE('',#1574,#1580,#1074,.T.);
#1938=EDGE_CURVE('',#1575,#1579,#1075,.T.);
#1939=EDGE_CURVE('',#1570,#1578,#1076,.T.);
#1940=EDGE_CURVE('',#1583,#1567,#1077,.T.);
#1941=EDGE_CURVE('',#1584,#1584,#866,.T.);
#1942=EDGE_CURVE('',#1584,#1576,#1078,.T.);
#1943=EDGE_CURVE('',#1585,#1585,#867,.T.);
#1944=EDGE_CURVE('',#1585,#1584,#1079,.T.);
#1945=EDGE_CURVE('',#1586,#1586,#868,.T.);
#1946=EDGE_CURVE('',#1586,#1587,#1080,.T.);
#1947=EDGE_CURVE('',#1587,#1587,#869,.T.);
#1948=EDGE_CURVE('',#1588,#1589,#1081,.T.);
#1949=EDGE_CURVE('',#1590,#1588,#1082,.T.);
#1950=EDGE_CURVE('',#1591,#1590,#1083,.T.);
#1951=EDGE_CURVE('',#1592,#1591,#1084,.T.);
#1952=EDGE_CURVE('',#1593,#1592,#1085,.T.);
#1953=EDGE_CURVE('',#1589,#1593,#1086,.T.);
#1954=EDGE_CURVE('',#1588,#1594,#1087,.T.);
#1955=EDGE_CURVE('',#1595,#1594,#1088,.T.);
#1956=EDGE_CURVE('',#1590,#1595,#1089,.T.);
#1957=EDGE_CURVE('',#1596,#1595,#1090,.T.);
#1958=EDGE_CURVE('',#1591,#1596,#1091,.T.);
#1959=EDGE_CURVE('',#1597,#1596,#1092,.T.);
#1960=EDGE_CURVE('',#1592,#1597,#1093,.T.);
#1961=EDGE_CURVE('',#1598,#1597,#1094,.T.);
#1962=EDGE_CURVE('',#1593,#1598,#1095,.T.);
#1963=EDGE_CURVE('',#1599,#1598,#1096,.T.);
#1964=EDGE_CURVE('',#1589,#1599,#1097,.T.);
#1965=EDGE_CURVE('',#1594,#1599,#1098,.T.);
#1966=EDGE_CURVE('',#1600,#1600,#870,.T.);
#1967=EDGE_CURVE('',#1600,#1601,#1099,.T.);
#1968=EDGE_CURVE('',#1601,#1601,#871,.T.);
#1969=EDGE_CURVE('',#1602,#1602,#872,.T.);
#1970=EDGE_CURVE('',#1603,#1604,#1100,.T.);
#1971=EDGE_CURVE('',#1604,#1605,#1101,.T.);
#1972=EDGE_CURVE('',#1605,#1606,#1102,.T.);
#1973=EDGE_CURVE('',#1606,#1607,#1103,.T.);
#1974=EDGE_CURVE('',#1607,#1608,#1104,.T.);
#1975=EDGE_CURVE('',#1608,#1603,#1105,.T.);
#1976=EDGE_CURVE('',#1609,#1609,#873,.T.);
#1977=EDGE_CURVE('',#1610,#1611,#1106,.T.);
#1978=EDGE_CURVE('',#1612,#1610,#1107,.T.);
#1979=EDGE_CURVE('',#1613,#1612,#1108,.T.);
#1980=EDGE_CURVE('',#1614,#1613,#1109,.T.);
#1981=EDGE_CURVE('',#1615,#1614,#1110,.T.);
#1982=EDGE_CURVE('',#1611,#1615,#1111,.T.);
#1983=EDGE_CURVE('',#1616,#1616,#874,.T.);
#1984=EDGE_CURVE('',#1610,#1603,#1112,.T.);
#1985=EDGE_CURVE('',#1612,#1608,#1113,.T.);
#1986=EDGE_CURVE('',#1613,#1607,#1114,.T.);
#1987=EDGE_CURVE('',#1614,#1606,#1115,.T.);
#1988=EDGE_CURVE('',#1615,#1605,#1116,.T.);
#1989=EDGE_CURVE('',#1611,#1604,#1117,.T.);
#1990=EDGE_CURVE('',#1617,#1617,#875,.T.);
#1991=EDGE_CURVE('',#1617,#1618,#1118,.T.);
#1992=EDGE_CURVE('',#1618,#1618,#876,.T.);
#1993=EDGE_CURVE('',#1619,#1619,#877,.T.);
#1994=EDGE_CURVE('',#1609,#1619,#1119,.T.);
#1995=EDGE_CURVE('',#1620,#1620,#878,.T.);
#1996=EDGE_CURVE('',#1620,#1616,#1120,.T.);
#1997=EDGE_CURVE('',#1621,#1621,#879,.T.);
#1998=EDGE_CURVE('',#1621,#1602,#1121,.T.);
#1999=EDGE_CURVE('',#1622,#1622,#880,.T.);
#2000=EDGE_CURVE('',#1623,#1623,#881,.T.);
#2001=EDGE_CURVE('',#1624,#1624,#882,.T.);
#2002=EDGE_CURVE('',#1624,#1622,#1122,.T.);
#2003=EDGE_CURVE('',#1625,#1625,#883,.T.);
#2004=EDGE_CURVE('',#1626,#1626,#884,.T.);
#2005=EDGE_CURVE('',#1626,#1625,#1123,.T.);
#2006=EDGE_CURVE('',#1627,#1627,#885,.T.);
#2007=EDGE_CURVE('',#1627,#1623,#1124,.T.);
#2008=EDGE_CURVE('',#1628,#1628,#886,.T.);
#2009=EDGE_CURVE('',#1629,#1629,#887,.T.);
#2010=EDGE_CURVE('',#1629,#1628,#1125,.T.);
#2011=EDGE_CURVE('',#1630,#1630,#888,.T.);
#2012=EDGE_CURVE('',#1630,#1629,#1126,.T.);
#2013=EDGE_CURVE('',#1631,#1631,#889,.T.);
#2014=EDGE_CURVE('',#1631,#1632,#1127,.T.);
#2015=EDGE_CURVE('',#1632,#1632,#890,.T.);
#2016=EDGE_CURVE('',#1633,#1633,#891,.T.);
#2017=EDGE_CURVE('',#1633,#1634,#1128,.T.);
#2018=EDGE_CURVE('',#1634,#1634,#892,.T.);
#2019=EDGE_CURVE('',#1635,#1635,#893,.F.);
#2020=EDGE_CURVE('',#1635,#1636,#1129,.T.);
#2021=EDGE_CURVE('',#1636,#1636,#894,.F.);
#2022=EDGE_CURVE('',#1637,#1637,#895,.T.);
#2023=EDGE_CURVE('',#1637,#1635,#1130,.T.);
#2024=EDGE_CURVE('',#1638,#1638,#896,.T.);
#2025=EDGE_CURVE('',#1638,#1639,#1131,.T.);
#2026=EDGE_CURVE('',#1640,#1639,#11,.T.);
#2027=EDGE_CURVE('',#1641,#1640,#12,.T.);
#2028=EDGE_CURVE('',#1642,#1641,#13,.T.);
#2029=EDGE_CURVE('',#1643,#1642,#14,.T.);
#2030=EDGE_CURVE('',#1644,#1643,#15,.T.);
#2031=EDGE_CURVE('',#1639,#1644,#16,.T.);
#2032=EDGE_CURVE('',#1645,#1643,#1132,.T.);
#2033=EDGE_CURVE('',#1645,#1646,#1133,.T.);
#2034=EDGE_CURVE('',#1646,#1644,#1134,.T.);
#2035=EDGE_CURVE('',#1647,#1642,#1135,.T.);
#2036=EDGE_CURVE('',#1647,#1645,#1136,.T.);
#2037=EDGE_CURVE('',#1648,#1641,#1137,.T.);
#2038=EDGE_CURVE('',#1648,#1647,#1138,.T.);
#2039=EDGE_CURVE('',#1649,#1640,#1139,.T.);
#2040=EDGE_CURVE('',#1649,#1648,#1140,.T.);
#2041=EDGE_CURVE('',#1650,#1639,#1141,.T.);
#2042=EDGE_CURVE('',#1650,#1649,#1142,.T.);
#2043=EDGE_CURVE('',#1646,#1650,#1143,.T.);
#2044=ORIENTED_EDGE('',*,*,#1651,.T.);
#2045=ORIENTED_EDGE('',*,*,#1652,.T.);
#2046=ORIENTED_EDGE('',*,*,#1653,.T.);
#2047=ORIENTED_EDGE('',*,*,#1654,.T.);
#2048=ORIENTED_EDGE('',*,*,#1652,.F.);
#2049=ORIENTED_EDGE('',*,*,#1655,.T.);
#2050=ORIENTED_EDGE('',*,*,#1656,.T.);
#2051=ORIENTED_EDGE('',*,*,#1657,.F.);
#2052=ORIENTED_EDGE('',*,*,#1656,.F.);
#2053=ORIENTED_EDGE('',*,*,#1658,.T.);
#2054=ORIENTED_EDGE('',*,*,#1659,.F.);
#2055=ORIENTED_EDGE('',*,*,#1660,.T.);
#2056=ORIENTED_EDGE('',*,*,#1661,.T.);
#2057=ORIENTED_EDGE('',*,*,#1662,.T.);
#2058=ORIENTED_EDGE('',*,*,#1663,.T.);
#2059=ORIENTED_EDGE('',*,*,#1664,.T.);
#2060=ORIENTED_EDGE('',*,*,#1665,.T.);
#2061=ORIENTED_EDGE('',*,*,#1666,.F.);
#2062=ORIENTED_EDGE('',*,*,#1665,.F.);
#2063=ORIENTED_EDGE('',*,*,#1667,.T.);
#2064=ORIENTED_EDGE('',*,*,#1668,.F.);
#2065=ORIENTED_EDGE('',*,*,#1669,.T.);
#2066=ORIENTED_EDGE('',*,*,#1670,.T.);
#2067=ORIENTED_EDGE('',*,*,#1671,.F.);
#2068=ORIENTED_EDGE('',*,*,#1672,.F.);
#2069=ORIENTED_EDGE('',*,*,#1673,.T.);
#2070=ORIENTED_EDGE('',*,*,#1674,.F.);
#2071=ORIENTED_EDGE('',*,*,#1675,.F.);
#2072=ORIENTED_EDGE('',*,*,#1673,.F.);
#2073=ORIENTED_EDGE('',*,*,#1676,.F.);
#2074=ORIENTED_EDGE('',*,*,#1677,.T.);
#2075=ORIENTED_EDGE('',*,*,#1678,.T.);
#2076=ORIENTED_EDGE('',*,*,#1677,.F.);
#2077=ORIENTED_EDGE('',*,*,#1678,.F.);
#2078=ORIENTED_EDGE('',*,*,#1679,.F.);
#2079=ORIENTED_EDGE('',*,*,#1680,.T.);
#2080=ORIENTED_EDGE('',*,*,#1681,.T.);
#2081=ORIENTED_EDGE('',*,*,#1680,.F.);
#2082=ORIENTED_EDGE('',*,*,#1681,.F.);
#2083=ORIENTED_EDGE('',*,*,#1682,.F.);
#2084=ORIENTED_EDGE('',*,*,#1683,.T.);
#2085=ORIENTED_EDGE('',*,*,#1684,.T.);
#2086=ORIENTED_EDGE('',*,*,#1683,.F.);
#2087=ORIENTED_EDGE('',*,*,#1684,.F.);
#2088=ORIENTED_EDGE('',*,*,#1676,.T.);
#2089=ORIENTED_EDGE('',*,*,#1685,.F.);
#2090=ORIENTED_EDGE('',*,*,#1686,.T.);
#2091=ORIENTED_EDGE('',*,*,#1687,.T.);
#2092=ORIENTED_EDGE('',*,*,#1686,.F.);
#2093=ORIENTED_EDGE('',*,*,#1687,.F.);
#2094=ORIENTED_EDGE('',*,*,#1679,.T.);
#2095=ORIENTED_EDGE('',*,*,#1688,.F.);
#2096=ORIENTED_EDGE('',*,*,#1689,.T.);
#2097=ORIENTED_EDGE('',*,*,#1690,.F.);
#2098=ORIENTED_EDGE('',*,*,#1691,.F.);
#2099=ORIENTED_EDGE('',*,*,#1689,.F.);
#2100=ORIENTED_EDGE('',*,*,#1692,.F.);
#2101=ORIENTED_EDGE('',*,*,#1693,.T.);
#2102=ORIENTED_EDGE('',*,*,#1694,.T.);
#2103=ORIENTED_EDGE('',*,*,#1693,.F.);
#2104=ORIENTED_EDGE('',*,*,#1694,.F.);
#2105=ORIENTED_EDGE('',*,*,#1695,.F.);
#2106=ORIENTED_EDGE('',*,*,#1696,.T.);
#2107=ORIENTED_EDGE('',*,*,#1697,.T.);
#2108=ORIENTED_EDGE('',*,*,#1696,.F.);
#2109=ORIENTED_EDGE('',*,*,#1697,.F.);
#2110=ORIENTED_EDGE('',*,*,#1698,.F.);
#2111=ORIENTED_EDGE('',*,*,#1699,.T.);
#2112=ORIENTED_EDGE('',*,*,#1700,.T.);
#2113=ORIENTED_EDGE('',*,*,#1699,.F.);
#2114=ORIENTED_EDGE('',*,*,#1700,.F.);
#2115=ORIENTED_EDGE('',*,*,#1692,.T.);
#2116=ORIENTED_EDGE('',*,*,#1701,.F.);
#2117=ORIENTED_EDGE('',*,*,#1702,.T.);
#2118=ORIENTED_EDGE('',*,*,#1703,.T.);
#2119=ORIENTED_EDGE('',*,*,#1702,.F.);
#2120=ORIENTED_EDGE('',*,*,#1703,.F.);
#2121=ORIENTED_EDGE('',*,*,#1695,.T.);
#2122=ORIENTED_EDGE('',*,*,#1704,.T.);
#2123=ORIENTED_EDGE('',*,*,#1659,.T.);
#2124=ORIENTED_EDGE('',*,*,#1705,.F.);
#2125=ORIENTED_EDGE('',*,*,#1706,.T.);
#2126=ORIENTED_EDGE('',*,*,#1664,.F.);
#2127=ORIENTED_EDGE('',*,*,#1707,.F.);
#2128=ORIENTED_EDGE('',*,*,#1670,.F.);
#2129=ORIENTED_EDGE('',*,*,#1708,.T.);
#2130=ORIENTED_EDGE('',*,*,#1709,.F.);
#2131=ORIENTED_EDGE('',*,*,#1710,.F.);
#2132=ORIENTED_EDGE('',*,*,#1711,.F.);
#2133=ORIENTED_EDGE('',*,*,#1712,.T.);
#2134=ORIENTED_EDGE('',*,*,#1713,.F.);
#2135=ORIENTED_EDGE('',*,*,#1714,.F.);
#2136=ORIENTED_EDGE('',*,*,#1715,.F.);
#2137=ORIENTED_EDGE('',*,*,#1716,.T.);
#2138=ORIENTED_EDGE('',*,*,#1655,.F.);
#2139=ORIENTED_EDGE('',*,*,#1651,.F.);
#2140=ORIENTED_EDGE('',*,*,#1654,.F.);
#2141=ORIENTED_EDGE('',*,*,#1717,.T.);
#2142=ORIENTED_EDGE('',*,*,#1718,.F.);
#2143=ORIENTED_EDGE('',*,*,#1717,.F.);
#2144=ORIENTED_EDGE('',*,*,#1653,.F.);
#2145=ORIENTED_EDGE('',*,*,#1704,.F.);
#2146=ORIENTED_EDGE('',*,*,#1658,.F.);
#2147=ORIENTED_EDGE('',*,*,#1716,.F.);
#2148=ORIENTED_EDGE('',*,*,#1719,.F.);
#2149=ORIENTED_EDGE('',*,*,#1660,.F.);
#2150=ORIENTED_EDGE('',*,*,#1720,.F.);
#2151=ORIENTED_EDGE('',*,*,#1712,.F.);
#2152=ORIENTED_EDGE('',*,*,#1721,.F.);
#2153=ORIENTED_EDGE('',*,*,#1662,.F.);
#2154=ORIENTED_EDGE('',*,*,#1722,.F.);
#2155=ORIENTED_EDGE('',*,*,#1708,.F.);
#2156=ORIENTED_EDGE('',*,*,#1669,.F.);
#2157=ORIENTED_EDGE('',*,*,#1723,.F.);
#2158=ORIENTED_EDGE('',*,*,#1667,.F.);
#2159=ORIENTED_EDGE('',*,*,#1706,.F.);
#2160=ORIENTED_EDGE('',*,*,#1690,.T.);
#2161=ORIENTED_EDGE('',*,*,#1691,.T.);
#2162=ORIENTED_EDGE('',*,*,#1674,.T.);
#2163=ORIENTED_EDGE('',*,*,#1675,.T.);
#2164=ORIENTED_EDGE('',*,*,#1714,.T.);
#2165=ORIENTED_EDGE('',*,*,#1724,.T.);
#2166=ORIENTED_EDGE('',*,*,#1713,.T.);
#2167=ORIENTED_EDGE('',*,*,#1725,.T.);
#2168=ORIENTED_EDGE('',*,*,#1726,.F.);
#2169=ORIENTED_EDGE('',*,*,#1725,.F.);
#2170=ORIENTED_EDGE('',*,*,#1720,.T.);
#2171=ORIENTED_EDGE('',*,*,#1661,.F.);
#2172=ORIENTED_EDGE('',*,*,#1719,.T.);
#2173=ORIENTED_EDGE('',*,*,#1715,.T.);
#2174=ORIENTED_EDGE('',*,*,#1724,.F.);
#2175=ORIENTED_EDGE('',*,*,#1710,.T.);
#2176=ORIENTED_EDGE('',*,*,#1727,.T.);
#2177=ORIENTED_EDGE('',*,*,#1709,.T.);
#2178=ORIENTED_EDGE('',*,*,#1728,.T.);
#2179=ORIENTED_EDGE('',*,*,#1729,.F.);
#2180=ORIENTED_EDGE('',*,*,#1728,.F.);
#2181=ORIENTED_EDGE('',*,*,#1722,.T.);
#2182=ORIENTED_EDGE('',*,*,#1663,.F.);
#2183=ORIENTED_EDGE('',*,*,#1721,.T.);
#2184=ORIENTED_EDGE('',*,*,#1711,.T.);
#2185=ORIENTED_EDGE('',*,*,#1727,.F.);
#2186=ORIENTED_EDGE('',*,*,#1707,.T.);
#2187=ORIENTED_EDGE('',*,*,#1671,.T.);
#2188=ORIENTED_EDGE('',*,*,#1723,.T.);
#2189=ORIENTED_EDGE('',*,*,#1668,.T.);
#2190=ORIENTED_EDGE('',*,*,#1730,.T.);
#2191=ORIENTED_EDGE('',*,*,#1731,.T.);
#2192=ORIENTED_EDGE('',*,*,#1732,.F.);
#2193=ORIENTED_EDGE('',*,*,#1733,.F.);
#2194=ORIENTED_EDGE('',*,*,#1734,.T.);
#2195=ORIENTED_EDGE('',*,*,#1733,.T.);
#2196=ORIENTED_EDGE('',*,*,#1735,.F.);
#2197=ORIENTED_EDGE('',*,*,#1736,.F.);
#2198=ORIENTED_EDGE('',*,*,#1718,.T.);
#2199=ORIENTED_EDGE('',*,*,#1737,.T.);
#2200=ORIENTED_EDGE('',*,*,#1736,.T.);
#2201=ORIENTED_EDGE('',*,*,#1738,.F.);
#2202=ORIENTED_EDGE('',*,*,#1739,.F.);
#2203=ORIENTED_EDGE('',*,*,#1740,.T.);
#2204=ORIENTED_EDGE('',*,*,#1739,.T.);
#2205=ORIENTED_EDGE('',*,*,#1741,.F.);
#2206=ORIENTED_EDGE('',*,*,#1731,.F.);
#2207=ORIENTED_EDGE('',*,*,#1705,.T.);
#2208=ORIENTED_EDGE('',*,*,#1741,.T.);
#2209=ORIENTED_EDGE('',*,*,#1738,.T.);
#2210=ORIENTED_EDGE('',*,*,#1735,.T.);
#2211=ORIENTED_EDGE('',*,*,#1732,.T.);
#2212=ORIENTED_EDGE('',*,*,#1657,.T.);
#2213=ORIENTED_EDGE('',*,*,#1726,.T.);
#2214=ORIENTED_EDGE('',*,*,#1729,.T.);
#2215=ORIENTED_EDGE('',*,*,#1666,.T.);
#2216=ORIENTED_EDGE('',*,*,#1740,.F.);
#2217=ORIENTED_EDGE('',*,*,#1730,.F.);
#2218=ORIENTED_EDGE('',*,*,#1734,.F.);
#2219=ORIENTED_EDGE('',*,*,#1737,.F.);
#2220=ORIENTED_EDGE('',*,*,#1672,.T.);
#2221=ORIENTED_EDGE('',*,*,#1682,.T.);
#2222=ORIENTED_EDGE('',*,*,#1685,.T.);
#2223=ORIENTED_EDGE('',*,*,#1688,.T.);
#2224=ORIENTED_EDGE('',*,*,#1698,.T.);
#2225=ORIENTED_EDGE('',*,*,#1701,.T.);
#2226=ORIENTED_EDGE('',*,*,#1742,.F.);
#2227=ORIENTED_EDGE('',*,*,#1743,.T.);
#2228=ORIENTED_EDGE('',*,*,#1744,.F.);
#2229=ORIENTED_EDGE('',*,*,#1743,.F.);
#2230=ORIENTED_EDGE('',*,*,#1742,.T.);
#2231=ORIENTED_EDGE('',*,*,#1745,.F.);
#2232=ORIENTED_EDGE('',*,*,#1746,.F.);
#2233=ORIENTED_EDGE('',*,*,#1747,.F.);
#2234=ORIENTED_EDGE('',*,*,#1748,.F.);
#2235=ORIENTED_EDGE('',*,*,#1749,.F.);
#2236=ORIENTED_EDGE('',*,*,#1750,.F.);
#2237=ORIENTED_EDGE('',*,*,#1751,.F.);
#2238=ORIENTED_EDGE('',*,*,#1752,.T.);
#2239=ORIENTED_EDGE('',*,*,#1747,.T.);
#2240=ORIENTED_EDGE('',*,*,#1753,.T.);
#2241=ORIENTED_EDGE('',*,*,#1754,.F.);
#2242=ORIENTED_EDGE('',*,*,#1755,.F.);
#2243=ORIENTED_EDGE('',*,*,#1748,.T.);
#2244=ORIENTED_EDGE('',*,*,#1755,.T.);
#2245=ORIENTED_EDGE('',*,*,#1756,.F.);
#2246=ORIENTED_EDGE('',*,*,#1757,.F.);
#2247=ORIENTED_EDGE('',*,*,#1749,.T.);
#2248=ORIENTED_EDGE('',*,*,#1757,.T.);
#2249=ORIENTED_EDGE('',*,*,#1758,.F.);
#2250=ORIENTED_EDGE('',*,*,#1759,.F.);
#2251=ORIENTED_EDGE('',*,*,#1750,.T.);
#2252=ORIENTED_EDGE('',*,*,#1759,.T.);
#2253=ORIENTED_EDGE('',*,*,#1760,.F.);
#2254=ORIENTED_EDGE('',*,*,#1761,.F.);
#2255=ORIENTED_EDGE('',*,*,#1751,.T.);
#2256=ORIENTED_EDGE('',*,*,#1761,.T.);
#2257=ORIENTED_EDGE('',*,*,#1762,.F.);
#2258=ORIENTED_EDGE('',*,*,#1763,.F.);
#2259=ORIENTED_EDGE('',*,*,#1746,.T.);
#2260=ORIENTED_EDGE('',*,*,#1763,.T.);
#2261=ORIENTED_EDGE('',*,*,#1764,.F.);
#2262=ORIENTED_EDGE('',*,*,#1753,.F.);
#2263=ORIENTED_EDGE('',*,*,#1764,.T.);
#2264=ORIENTED_EDGE('',*,*,#1762,.T.);
#2265=ORIENTED_EDGE('',*,*,#1760,.T.);
#2266=ORIENTED_EDGE('',*,*,#1758,.T.);
#2267=ORIENTED_EDGE('',*,*,#1756,.T.);
#2268=ORIENTED_EDGE('',*,*,#1754,.T.);
#2269=ORIENTED_EDGE('',*,*,#1744,.T.);
#2270=ORIENTED_EDGE('',*,*,#1745,.T.);
#2271=ORIENTED_EDGE('',*,*,#1765,.T.);
#2272=ORIENTED_EDGE('',*,*,#1766,.T.);
#2273=ORIENTED_EDGE('',*,*,#1765,.F.);
#2274=ORIENTED_EDGE('',*,*,#1752,.F.);
#2275=ORIENTED_EDGE('',*,*,#1767,.T.);
#2276=ORIENTED_EDGE('',*,*,#1768,.T.);
#2277=ORIENTED_EDGE('',*,*,#1767,.F.);
#2278=ORIENTED_EDGE('',*,*,#1768,.F.);
#2279=ORIENTED_EDGE('',*,*,#1766,.F.);
#2280=ORIENTED_EDGE('',*,*,#1769,.F.);
#2281=ORIENTED_EDGE('',*,*,#1770,.T.);
#2282=ORIENTED_EDGE('',*,*,#1771,.F.);
#2283=ORIENTED_EDGE('',*,*,#1770,.F.);
#2284=ORIENTED_EDGE('',*,*,#1769,.T.);
#2285=ORIENTED_EDGE('',*,*,#1772,.F.);
#2286=ORIENTED_EDGE('',*,*,#1773,.F.);
#2287=ORIENTED_EDGE('',*,*,#1774,.F.);
#2288=ORIENTED_EDGE('',*,*,#1775,.F.);
#2289=ORIENTED_EDGE('',*,*,#1776,.F.);
#2290=ORIENTED_EDGE('',*,*,#1777,.F.);
#2291=ORIENTED_EDGE('',*,*,#1778,.F.);
#2292=ORIENTED_EDGE('',*,*,#1779,.T.);
#2293=ORIENTED_EDGE('',*,*,#1774,.T.);
#2294=ORIENTED_EDGE('',*,*,#1780,.T.);
#2295=ORIENTED_EDGE('',*,*,#1781,.F.);
#2296=ORIENTED_EDGE('',*,*,#1782,.F.);
#2297=ORIENTED_EDGE('',*,*,#1775,.T.);
#2298=ORIENTED_EDGE('',*,*,#1782,.T.);
#2299=ORIENTED_EDGE('',*,*,#1783,.F.);
#2300=ORIENTED_EDGE('',*,*,#1784,.F.);
#2301=ORIENTED_EDGE('',*,*,#1776,.T.);
#2302=ORIENTED_EDGE('',*,*,#1784,.T.);
#2303=ORIENTED_EDGE('',*,*,#1785,.F.);
#2304=ORIENTED_EDGE('',*,*,#1786,.F.);
#2305=ORIENTED_EDGE('',*,*,#1777,.T.);
#2306=ORIENTED_EDGE('',*,*,#1786,.T.);
#2307=ORIENTED_EDGE('',*,*,#1787,.F.);
#2308=ORIENTED_EDGE('',*,*,#1788,.F.);
#2309=ORIENTED_EDGE('',*,*,#1778,.T.);
#2310=ORIENTED_EDGE('',*,*,#1788,.T.);
#2311=ORIENTED_EDGE('',*,*,#1789,.F.);
#2312=ORIENTED_EDGE('',*,*,#1790,.F.);
#2313=ORIENTED_EDGE('',*,*,#1773,.T.);
#2314=ORIENTED_EDGE('',*,*,#1790,.T.);
#2315=ORIENTED_EDGE('',*,*,#1791,.F.);
#2316=ORIENTED_EDGE('',*,*,#1780,.F.);
#2317=ORIENTED_EDGE('',*,*,#1791,.T.);
#2318=ORIENTED_EDGE('',*,*,#1789,.T.);
#2319=ORIENTED_EDGE('',*,*,#1787,.T.);
#2320=ORIENTED_EDGE('',*,*,#1785,.T.);
#2321=ORIENTED_EDGE('',*,*,#1783,.T.);
#2322=ORIENTED_EDGE('',*,*,#1781,.T.);
#2323=ORIENTED_EDGE('',*,*,#1771,.T.);
#2324=ORIENTED_EDGE('',*,*,#1772,.T.);
#2325=ORIENTED_EDGE('',*,*,#1792,.T.);
#2326=ORIENTED_EDGE('',*,*,#1793,.T.);
#2327=ORIENTED_EDGE('',*,*,#1792,.F.);
#2328=ORIENTED_EDGE('',*,*,#1779,.F.);
#2329=ORIENTED_EDGE('',*,*,#1794,.T.);
#2330=ORIENTED_EDGE('',*,*,#1795,.T.);
#2331=ORIENTED_EDGE('',*,*,#1794,.F.);
#2332=ORIENTED_EDGE('',*,*,#1795,.F.);
#2333=ORIENTED_EDGE('',*,*,#1793,.F.);
#2334=ORIENTED_EDGE('',*,*,#1796,.F.);
#2335=ORIENTED_EDGE('',*,*,#1797,.T.);
#2336=ORIENTED_EDGE('',*,*,#1798,.F.);
#2337=ORIENTED_EDGE('',*,*,#1797,.F.);
#2338=ORIENTED_EDGE('',*,*,#1796,.T.);
#2339=ORIENTED_EDGE('',*,*,#1799,.F.);
#2340=ORIENTED_EDGE('',*,*,#1800,.F.);
#2341=ORIENTED_EDGE('',*,*,#1801,.F.);
#2342=ORIENTED_EDGE('',*,*,#1802,.F.);
#2343=ORIENTED_EDGE('',*,*,#1803,.F.);
#2344=ORIENTED_EDGE('',*,*,#1804,.F.);
#2345=ORIENTED_EDGE('',*,*,#1805,.F.);
#2346=ORIENTED_EDGE('',*,*,#1806,.T.);
#2347=ORIENTED_EDGE('',*,*,#1801,.T.);
#2348=ORIENTED_EDGE('',*,*,#1807,.T.);
#2349=ORIENTED_EDGE('',*,*,#1808,.F.);
#2350=ORIENTED_EDGE('',*,*,#1809,.F.);
#2351=ORIENTED_EDGE('',*,*,#1802,.T.);
#2352=ORIENTED_EDGE('',*,*,#1809,.T.);
#2353=ORIENTED_EDGE('',*,*,#1810,.F.);
#2354=ORIENTED_EDGE('',*,*,#1811,.F.);
#2355=ORIENTED_EDGE('',*,*,#1803,.T.);
#2356=ORIENTED_EDGE('',*,*,#1811,.T.);
#2357=ORIENTED_EDGE('',*,*,#1812,.F.);
#2358=ORIENTED_EDGE('',*,*,#1813,.F.);
#2359=ORIENTED_EDGE('',*,*,#1804,.T.);
#2360=ORIENTED_EDGE('',*,*,#1813,.T.);
#2361=ORIENTED_EDGE('',*,*,#1814,.F.);
#2362=ORIENTED_EDGE('',*,*,#1815,.F.);
#2363=ORIENTED_EDGE('',*,*,#1805,.T.);
#2364=ORIENTED_EDGE('',*,*,#1815,.T.);
#2365=ORIENTED_EDGE('',*,*,#1816,.F.);
#2366=ORIENTED_EDGE('',*,*,#1817,.F.);
#2367=ORIENTED_EDGE('',*,*,#1800,.T.);
#2368=ORIENTED_EDGE('',*,*,#1817,.T.);
#2369=ORIENTED_EDGE('',*,*,#1818,.F.);
#2370=ORIENTED_EDGE('',*,*,#1807,.F.);
#2371=ORIENTED_EDGE('',*,*,#1818,.T.);
#2372=ORIENTED_EDGE('',*,*,#1816,.T.);
#2373=ORIENTED_EDGE('',*,*,#1814,.T.);
#2374=ORIENTED_EDGE('',*,*,#1812,.T.);
#2375=ORIENTED_EDGE('',*,*,#1810,.T.);
#2376=ORIENTED_EDGE('',*,*,#1808,.T.);
#2377=ORIENTED_EDGE('',*,*,#1798,.T.);
#2378=ORIENTED_EDGE('',*,*,#1799,.T.);
#2379=ORIENTED_EDGE('',*,*,#1819,.T.);
#2380=ORIENTED_EDGE('',*,*,#1820,.T.);
#2381=ORIENTED_EDGE('',*,*,#1819,.F.);
#2382=ORIENTED_EDGE('',*,*,#1806,.F.);
#2383=ORIENTED_EDGE('',*,*,#1821,.T.);
#2384=ORIENTED_EDGE('',*,*,#1822,.T.);
#2385=ORIENTED_EDGE('',*,*,#1821,.F.);
#2386=ORIENTED_EDGE('',*,*,#1822,.F.);
#2387=ORIENTED_EDGE('',*,*,#1820,.F.);
#2388=ORIENTED_EDGE('',*,*,#1823,.F.);
#2389=ORIENTED_EDGE('',*,*,#1824,.T.);
#2390=ORIENTED_EDGE('',*,*,#1825,.F.);
#2391=ORIENTED_EDGE('',*,*,#1824,.F.);
#2392=ORIENTED_EDGE('',*,*,#1823,.T.);
#2393=ORIENTED_EDGE('',*,*,#1826,.F.);
#2394=ORIENTED_EDGE('',*,*,#1827,.F.);
#2395=ORIENTED_EDGE('',*,*,#1828,.F.);
#2396=ORIENTED_EDGE('',*,*,#1829,.F.);
#2397=ORIENTED_EDGE('',*,*,#1830,.F.);
#2398=ORIENTED_EDGE('',*,*,#1831,.F.);
#2399=ORIENTED_EDGE('',*,*,#1832,.F.);
#2400=ORIENTED_EDGE('',*,*,#1833,.T.);
#2401=ORIENTED_EDGE('',*,*,#1828,.T.);
#2402=ORIENTED_EDGE('',*,*,#1834,.T.);
#2403=ORIENTED_EDGE('',*,*,#1835,.F.);
#2404=ORIENTED_EDGE('',*,*,#1836,.F.);
#2405=ORIENTED_EDGE('',*,*,#1829,.T.);
#2406=ORIENTED_EDGE('',*,*,#1836,.T.);
#2407=ORIENTED_EDGE('',*,*,#1837,.F.);
#2408=ORIENTED_EDGE('',*,*,#1838,.F.);
#2409=ORIENTED_EDGE('',*,*,#1830,.T.);
#2410=ORIENTED_EDGE('',*,*,#1838,.T.);
#2411=ORIENTED_EDGE('',*,*,#1839,.F.);
#2412=ORIENTED_EDGE('',*,*,#1840,.F.);
#2413=ORIENTED_EDGE('',*,*,#1831,.T.);
#2414=ORIENTED_EDGE('',*,*,#1840,.T.);
#2415=ORIENTED_EDGE('',*,*,#1841,.F.);
#2416=ORIENTED_EDGE('',*,*,#1842,.F.);
#2417=ORIENTED_EDGE('',*,*,#1832,.T.);
#2418=ORIENTED_EDGE('',*,*,#1842,.T.);
#2419=ORIENTED_EDGE('',*,*,#1843,.F.);
#2420=ORIENTED_EDGE('',*,*,#1844,.F.);
#2421=ORIENTED_EDGE('',*,*,#1827,.T.);
#2422=ORIENTED_EDGE('',*,*,#1844,.T.);
#2423=ORIENTED_EDGE('',*,*,#1845,.F.);
#2424=ORIENTED_EDGE('',*,*,#1834,.F.);
#2425=ORIENTED_EDGE('',*,*,#1845,.T.);
#2426=ORIENTED_EDGE('',*,*,#1843,.T.);
#2427=ORIENTED_EDGE('',*,*,#1841,.T.);
#2428=ORIENTED_EDGE('',*,*,#1839,.T.);
#2429=ORIENTED_EDGE('',*,*,#1837,.T.);
#2430=ORIENTED_EDGE('',*,*,#1835,.T.);
#2431=ORIENTED_EDGE('',*,*,#1825,.T.);
#2432=ORIENTED_EDGE('',*,*,#1826,.T.);
#2433=ORIENTED_EDGE('',*,*,#1846,.T.);
#2434=ORIENTED_EDGE('',*,*,#1847,.T.);
#2435=ORIENTED_EDGE('',*,*,#1846,.F.);
#2436=ORIENTED_EDGE('',*,*,#1833,.F.);
#2437=ORIENTED_EDGE('',*,*,#1848,.T.);
#2438=ORIENTED_EDGE('',*,*,#1849,.T.);
#2439=ORIENTED_EDGE('',*,*,#1848,.F.);
#2440=ORIENTED_EDGE('',*,*,#1849,.F.);
#2441=ORIENTED_EDGE('',*,*,#1847,.F.);
#2442=ORIENTED_EDGE('',*,*,#1850,.F.);
#2443=ORIENTED_EDGE('',*,*,#1851,.T.);
#2444=ORIENTED_EDGE('',*,*,#1852,.F.);
#2445=ORIENTED_EDGE('',*,*,#1851,.F.);
#2446=ORIENTED_EDGE('',*,*,#1853,.F.);
#2447=ORIENTED_EDGE('',*,*,#1854,.T.);
#2448=ORIENTED_EDGE('',*,*,#1855,.F.);
#2449=ORIENTED_EDGE('',*,*,#1854,.F.);
#2450=ORIENTED_EDGE('',*,*,#1856,.F.);
#2451=ORIENTED_EDGE('',*,*,#1857,.T.);
#2452=ORIENTED_EDGE('',*,*,#1858,.F.);
#2453=ORIENTED_EDGE('',*,*,#1857,.F.);
#2454=ORIENTED_EDGE('',*,*,#1859,.F.);
#2455=ORIENTED_EDGE('',*,*,#1860,.T.);
#2456=ORIENTED_EDGE('',*,*,#1861,.T.);
#2457=ORIENTED_EDGE('',*,*,#1860,.F.);
#2458=ORIENTED_EDGE('',*,*,#1861,.F.);
#2459=ORIENTED_EDGE('',*,*,#1862,.F.);
#2460=ORIENTED_EDGE('',*,*,#1863,.F.);
#2461=ORIENTED_EDGE('',*,*,#1864,.T.);
#2462=ORIENTED_EDGE('',*,*,#1865,.T.);
#2463=ORIENTED_EDGE('',*,*,#1864,.F.);
#2464=ORIENTED_EDGE('',*,*,#1865,.F.);
#2465=ORIENTED_EDGE('',*,*,#1866,.F.);
#2466=ORIENTED_EDGE('',*,*,#1862,.T.);
#2467=ORIENTED_EDGE('',*,*,#1867,.T.);
#2468=ORIENTED_EDGE('',*,*,#1868,.F.);
#2469=ORIENTED_EDGE('',*,*,#1867,.F.);
#2470=ORIENTED_EDGE('',*,*,#1866,.T.);
#2471=ORIENTED_EDGE('',*,*,#1869,.T.);
#2472=ORIENTED_EDGE('',*,*,#1870,.F.);
#2473=ORIENTED_EDGE('',*,*,#1869,.F.);
#2474=ORIENTED_EDGE('',*,*,#1871,.T.);
#2475=ORIENTED_EDGE('',*,*,#1872,.T.);
#2476=ORIENTED_EDGE('',*,*,#1873,.F.);
#2477=ORIENTED_EDGE('',*,*,#1874,.F.);
#2478=ORIENTED_EDGE('',*,*,#1875,.T.);
#2479=ORIENTED_EDGE('',*,*,#1874,.T.);
#2480=ORIENTED_EDGE('',*,*,#1876,.F.);
#2481=ORIENTED_EDGE('',*,*,#1877,.F.);
#2482=ORIENTED_EDGE('',*,*,#1878,.T.);
#2483=ORIENTED_EDGE('',*,*,#1877,.T.);
#2484=ORIENTED_EDGE('',*,*,#1879,.F.);
#2485=ORIENTED_EDGE('',*,*,#1880,.F.);
#2486=ORIENTED_EDGE('',*,*,#1881,.T.);
#2487=ORIENTED_EDGE('',*,*,#1880,.T.);
#2488=ORIENTED_EDGE('',*,*,#1882,.F.);
#2489=ORIENTED_EDGE('',*,*,#1872,.F.);
#2490=ORIENTED_EDGE('',*,*,#1882,.T.);
#2491=ORIENTED_EDGE('',*,*,#1879,.T.);
#2492=ORIENTED_EDGE('',*,*,#1876,.T.);
#2493=ORIENTED_EDGE('',*,*,#1873,.T.);
#2494=ORIENTED_EDGE('',*,*,#1852,.T.);
#2495=ORIENTED_EDGE('',*,*,#1855,.T.);
#2496=ORIENTED_EDGE('',*,*,#1858,.T.);
#2497=ORIENTED_EDGE('',*,*,#1868,.T.);
#2498=ORIENTED_EDGE('',*,*,#1870,.T.);
#2499=ORIENTED_EDGE('',*,*,#1881,.F.);
#2500=ORIENTED_EDGE('',*,*,#1871,.F.);
#2501=ORIENTED_EDGE('',*,*,#1875,.F.);
#2502=ORIENTED_EDGE('',*,*,#1878,.F.);
#2503=ORIENTED_EDGE('',*,*,#1850,.T.);
#2504=ORIENTED_EDGE('',*,*,#1853,.T.);
#2505=ORIENTED_EDGE('',*,*,#1856,.T.);
#2506=ORIENTED_EDGE('',*,*,#1859,.T.);
#2507=ORIENTED_EDGE('',*,*,#1863,.T.);
#2508=ORIENTED_EDGE('',*,*,#1883,.F.);
#2509=ORIENTED_EDGE('',*,*,#1884,.T.);
#2510=ORIENTED_EDGE('',*,*,#1885,.F.);
#2511=ORIENTED_EDGE('',*,*,#1884,.F.);
#2512=ORIENTED_EDGE('',*,*,#1886,.F.);
#2513=ORIENTED_EDGE('',*,*,#1887,.T.);
#2514=ORIENTED_EDGE('',*,*,#1888,.F.);
#2515=ORIENTED_EDGE('',*,*,#1887,.F.);
#2516=ORIENTED_EDGE('',*,*,#1889,.F.);
#2517=ORIENTED_EDGE('',*,*,#1890,.T.);
#2518=ORIENTED_EDGE('',*,*,#1891,.F.);
#2519=ORIENTED_EDGE('',*,*,#1890,.F.);
#2520=ORIENTED_EDGE('',*,*,#1892,.F.);
#2521=ORIENTED_EDGE('',*,*,#1893,.T.);
#2522=ORIENTED_EDGE('',*,*,#1894,.T.);
#2523=ORIENTED_EDGE('',*,*,#1893,.F.);
#2524=ORIENTED_EDGE('',*,*,#1894,.F.);
#2525=ORIENTED_EDGE('',*,*,#1895,.F.);
#2526=ORIENTED_EDGE('',*,*,#1896,.F.);
#2527=ORIENTED_EDGE('',*,*,#1897,.T.);
#2528=ORIENTED_EDGE('',*,*,#1898,.T.);
#2529=ORIENTED_EDGE('',*,*,#1897,.F.);
#2530=ORIENTED_EDGE('',*,*,#1898,.F.);
#2531=ORIENTED_EDGE('',*,*,#1899,.F.);
#2532=ORIENTED_EDGE('',*,*,#1895,.T.);
#2533=ORIENTED_EDGE('',*,*,#1900,.T.);
#2534=ORIENTED_EDGE('',*,*,#1901,.F.);
#2535=ORIENTED_EDGE('',*,*,#1900,.F.);
#2536=ORIENTED_EDGE('',*,*,#1899,.T.);
#2537=ORIENTED_EDGE('',*,*,#1902,.T.);
#2538=ORIENTED_EDGE('',*,*,#1903,.F.);
#2539=ORIENTED_EDGE('',*,*,#1902,.F.);
#2540=ORIENTED_EDGE('',*,*,#1904,.T.);
#2541=ORIENTED_EDGE('',*,*,#1905,.T.);
#2542=ORIENTED_EDGE('',*,*,#1906,.F.);
#2543=ORIENTED_EDGE('',*,*,#1907,.F.);
#2544=ORIENTED_EDGE('',*,*,#1908,.T.);
#2545=ORIENTED_EDGE('',*,*,#1907,.T.);
#2546=ORIENTED_EDGE('',*,*,#1909,.F.);
#2547=ORIENTED_EDGE('',*,*,#1910,.F.);
#2548=ORIENTED_EDGE('',*,*,#1911,.T.);
#2549=ORIENTED_EDGE('',*,*,#1910,.T.);
#2550=ORIENTED_EDGE('',*,*,#1912,.F.);
#2551=ORIENTED_EDGE('',*,*,#1913,.F.);
#2552=ORIENTED_EDGE('',*,*,#1914,.T.);
#2553=ORIENTED_EDGE('',*,*,#1913,.T.);
#2554=ORIENTED_EDGE('',*,*,#1915,.F.);
#2555=ORIENTED_EDGE('',*,*,#1905,.F.);
#2556=ORIENTED_EDGE('',*,*,#1915,.T.);
#2557=ORIENTED_EDGE('',*,*,#1912,.T.);
#2558=ORIENTED_EDGE('',*,*,#1909,.T.);
#2559=ORIENTED_EDGE('',*,*,#1906,.T.);
#2560=ORIENTED_EDGE('',*,*,#1885,.T.);
#2561=ORIENTED_EDGE('',*,*,#1888,.T.);
#2562=ORIENTED_EDGE('',*,*,#1891,.T.);
#2563=ORIENTED_EDGE('',*,*,#1901,.T.);
#2564=ORIENTED_EDGE('',*,*,#1903,.T.);
#2565=ORIENTED_EDGE('',*,*,#1914,.F.);
#2566=ORIENTED_EDGE('',*,*,#1904,.F.);
#2567=ORIENTED_EDGE('',*,*,#1908,.F.);
#2568=ORIENTED_EDGE('',*,*,#1911,.F.);
#2569=ORIENTED_EDGE('',*,*,#1883,.T.);
#2570=ORIENTED_EDGE('',*,*,#1886,.T.);
#2571=ORIENTED_EDGE('',*,*,#1889,.T.);
#2572=ORIENTED_EDGE('',*,*,#1892,.T.);
#2573=ORIENTED_EDGE('',*,*,#1896,.T.);
#2574=ORIENTED_EDGE('',*,*,#1916,.F.);
#2575=ORIENTED_EDGE('',*,*,#1917,.F.);
#2576=ORIENTED_EDGE('',*,*,#1918,.T.);
#2577=ORIENTED_EDGE('',*,*,#1919,.T.);
#2578=ORIENTED_EDGE('',*,*,#1917,.T.);
#2579=ORIENTED_EDGE('',*,*,#1919,.F.);
#2580=ORIENTED_EDGE('',*,*,#1920,.T.);
#2581=ORIENTED_EDGE('',*,*,#1921,.T.);
#2582=ORIENTED_EDGE('',*,*,#1922,.T.);
#2583=ORIENTED_EDGE('',*,*,#1923,.T.);
#2584=ORIENTED_EDGE('',*,*,#1924,.T.);
#2585=ORIENTED_EDGE('',*,*,#1925,.T.);
#2586=ORIENTED_EDGE('',*,*,#1926,.F.);
#2587=ORIENTED_EDGE('',*,*,#1927,.T.);
#2588=ORIENTED_EDGE('',*,*,#1928,.T.);
#2589=ORIENTED_EDGE('',*,*,#1929,.T.);
#2590=ORIENTED_EDGE('',*,*,#1930,.T.);
#2591=ORIENTED_EDGE('',*,*,#1931,.T.);
#2592=ORIENTED_EDGE('',*,*,#1932,.T.);
#2593=ORIENTED_EDGE('',*,*,#1933,.F.);
#2594=ORIENTED_EDGE('',*,*,#1934,.F.);
#2595=ORIENTED_EDGE('',*,*,#1932,.F.);
#2596=ORIENTED_EDGE('',*,*,#1935,.F.);
#2597=ORIENTED_EDGE('',*,*,#1921,.F.);
#2598=ORIENTED_EDGE('',*,*,#1935,.T.);
#2599=ORIENTED_EDGE('',*,*,#1931,.F.);
#2600=ORIENTED_EDGE('',*,*,#1936,.F.);
#2601=ORIENTED_EDGE('',*,*,#1922,.F.);
#2602=ORIENTED_EDGE('',*,*,#1936,.T.);
#2603=ORIENTED_EDGE('',*,*,#1930,.F.);
#2604=ORIENTED_EDGE('',*,*,#1937,.F.);
#2605=ORIENTED_EDGE('',*,*,#1923,.F.);
#2606=ORIENTED_EDGE('',*,*,#1937,.T.);
#2607=ORIENTED_EDGE('',*,*,#1929,.F.);
#2608=ORIENTED_EDGE('',*,*,#1938,.F.);
#2609=ORIENTED_EDGE('',*,*,#1924,.F.);
#2610=ORIENTED_EDGE('',*,*,#1938,.T.);
#2611=ORIENTED_EDGE('',*,*,#1928,.F.);
#2612=ORIENTED_EDGE('',*,*,#1939,.F.);
#2613=ORIENTED_EDGE('',*,*,#1925,.F.);
#2614=ORIENTED_EDGE('',*,*,#1939,.T.);
#2615=ORIENTED_EDGE('',*,*,#1927,.F.);
#2616=ORIENTED_EDGE('',*,*,#1934,.T.);
#2617=ORIENTED_EDGE('',*,*,#1920,.F.);
#2618=ORIENTED_EDGE('',*,*,#1933,.T.);
#2619=ORIENTED_EDGE('',*,*,#1940,.T.);
#2620=ORIENTED_EDGE('',*,*,#1916,.T.);
#2621=ORIENTED_EDGE('',*,*,#1940,.F.);
#2622=ORIENTED_EDGE('',*,*,#1941,.F.);
#2623=ORIENTED_EDGE('',*,*,#1942,.T.);
#2624=ORIENTED_EDGE('',*,*,#1926,.T.);
#2625=ORIENTED_EDGE('',*,*,#1942,.F.);
#2626=ORIENTED_EDGE('',*,*,#1943,.F.);
#2627=ORIENTED_EDGE('',*,*,#1944,.T.);
#2628=ORIENTED_EDGE('',*,*,#1941,.T.);
#2629=ORIENTED_EDGE('',*,*,#1944,.F.);
#2630=ORIENTED_EDGE('',*,*,#1943,.T.);
#2631=ORIENTED_EDGE('',*,*,#1918,.F.);
#2632=ORIENTED_EDGE('',*,*,#1945,.F.);
#2633=ORIENTED_EDGE('',*,*,#1946,.T.);
#2634=ORIENTED_EDGE('',*,*,#1947,.T.);
#2635=ORIENTED_EDGE('',*,*,#1946,.F.);
#2636=ORIENTED_EDGE('',*,*,#1947,.F.);
#2637=ORIENTED_EDGE('',*,*,#1948,.F.);
#2638=ORIENTED_EDGE('',*,*,#1949,.F.);
#2639=ORIENTED_EDGE('',*,*,#1950,.F.);
#2640=ORIENTED_EDGE('',*,*,#1951,.F.);
#2641=ORIENTED_EDGE('',*,*,#1952,.F.);
#2642=ORIENTED_EDGE('',*,*,#1953,.F.);
#2643=ORIENTED_EDGE('',*,*,#1945,.T.);
#2644=ORIENTED_EDGE('',*,*,#1949,.T.);
#2645=ORIENTED_EDGE('',*,*,#1954,.T.);
#2646=ORIENTED_EDGE('',*,*,#1955,.F.);
#2647=ORIENTED_EDGE('',*,*,#1956,.F.);
#2648=ORIENTED_EDGE('',*,*,#1950,.T.);
#2649=ORIENTED_EDGE('',*,*,#1956,.T.);
#2650=ORIENTED_EDGE('',*,*,#1957,.F.);
#2651=ORIENTED_EDGE('',*,*,#1958,.F.);
#2652=ORIENTED_EDGE('',*,*,#1951,.T.);
#2653=ORIENTED_EDGE('',*,*,#1958,.T.);
#2654=ORIENTED_EDGE('',*,*,#1959,.F.);
#2655=ORIENTED_EDGE('',*,*,#1960,.F.);
#2656=ORIENTED_EDGE('',*,*,#1952,.T.);
#2657=ORIENTED_EDGE('',*,*,#1960,.T.);
#2658=ORIENTED_EDGE('',*,*,#1961,.F.);
#2659=ORIENTED_EDGE('',*,*,#1962,.F.);
#2660=ORIENTED_EDGE('',*,*,#1953,.T.);
#2661=ORIENTED_EDGE('',*,*,#1962,.T.);
#2662=ORIENTED_EDGE('',*,*,#1963,.F.);
#2663=ORIENTED_EDGE('',*,*,#1964,.F.);
#2664=ORIENTED_EDGE('',*,*,#1948,.T.);
#2665=ORIENTED_EDGE('',*,*,#1964,.T.);
#2666=ORIENTED_EDGE('',*,*,#1965,.F.);
#2667=ORIENTED_EDGE('',*,*,#1954,.F.);
#2668=ORIENTED_EDGE('',*,*,#1965,.T.);
#2669=ORIENTED_EDGE('',*,*,#1963,.T.);
#2670=ORIENTED_EDGE('',*,*,#1961,.T.);
#2671=ORIENTED_EDGE('',*,*,#1959,.T.);
#2672=ORIENTED_EDGE('',*,*,#1957,.T.);
#2673=ORIENTED_EDGE('',*,*,#1955,.T.);
#2674=ORIENTED_EDGE('',*,*,#1966,.F.);
#2675=ORIENTED_EDGE('',*,*,#1967,.T.);
#2676=ORIENTED_EDGE('',*,*,#1968,.F.);
#2677=ORIENTED_EDGE('',*,*,#1967,.F.);
#2678=ORIENTED_EDGE('',*,*,#1966,.T.);
#2679=ORIENTED_EDGE('',*,*,#1969,.F.);
#2680=ORIENTED_EDGE('',*,*,#1970,.T.);
#2681=ORIENTED_EDGE('',*,*,#1971,.T.);
#2682=ORIENTED_EDGE('',*,*,#1972,.T.);
#2683=ORIENTED_EDGE('',*,*,#1973,.T.);
#2684=ORIENTED_EDGE('',*,*,#1974,.T.);
#2685=ORIENTED_EDGE('',*,*,#1975,.T.);
#2686=ORIENTED_EDGE('',*,*,#1976,.T.);
#2687=ORIENTED_EDGE('',*,*,#1977,.F.);
#2688=ORIENTED_EDGE('',*,*,#1978,.F.);
#2689=ORIENTED_EDGE('',*,*,#1979,.F.);
#2690=ORIENTED_EDGE('',*,*,#1980,.F.);
#2691=ORIENTED_EDGE('',*,*,#1981,.F.);
#2692=ORIENTED_EDGE('',*,*,#1982,.F.);
#2693=ORIENTED_EDGE('',*,*,#1983,.F.);
#2694=ORIENTED_EDGE('',*,*,#1978,.T.);
#2695=ORIENTED_EDGE('',*,*,#1984,.T.);
#2696=ORIENTED_EDGE('',*,*,#1975,.F.);
#2697=ORIENTED_EDGE('',*,*,#1985,.F.);
#2698=ORIENTED_EDGE('',*,*,#1979,.T.);
#2699=ORIENTED_EDGE('',*,*,#1985,.T.);
#2700=ORIENTED_EDGE('',*,*,#1974,.F.);
#2701=ORIENTED_EDGE('',*,*,#1986,.F.);
#2702=ORIENTED_EDGE('',*,*,#1980,.T.);
#2703=ORIENTED_EDGE('',*,*,#1986,.T.);
#2704=ORIENTED_EDGE('',*,*,#1973,.F.);
#2705=ORIENTED_EDGE('',*,*,#1987,.F.);
#2706=ORIENTED_EDGE('',*,*,#1981,.T.);
#2707=ORIENTED_EDGE('',*,*,#1987,.T.);
#2708=ORIENTED_EDGE('',*,*,#1972,.F.);
#2709=ORIENTED_EDGE('',*,*,#1988,.F.);
#2710=ORIENTED_EDGE('',*,*,#1982,.T.);
#2711=ORIENTED_EDGE('',*,*,#1988,.T.);
#2712=ORIENTED_EDGE('',*,*,#1971,.F.);
#2713=ORIENTED_EDGE('',*,*,#1989,.F.);
#2714=ORIENTED_EDGE('',*,*,#1977,.T.);
#2715=ORIENTED_EDGE('',*,*,#1989,.T.);
#2716=ORIENTED_EDGE('',*,*,#1970,.F.);
#2717=ORIENTED_EDGE('',*,*,#1984,.F.);
#2718=ORIENTED_EDGE('',*,*,#1990,.F.);
#2719=ORIENTED_EDGE('',*,*,#1968,.T.);
#2720=ORIENTED_EDGE('',*,*,#1990,.T.);
#2721=ORIENTED_EDGE('',*,*,#1991,.T.);
#2722=ORIENTED_EDGE('',*,*,#1992,.F.);
#2723=ORIENTED_EDGE('',*,*,#1991,.F.);
#2724=ORIENTED_EDGE('',*,*,#1993,.F.);
#2725=ORIENTED_EDGE('',*,*,#1992,.T.);
#2726=ORIENTED_EDGE('',*,*,#1976,.F.);
#2727=ORIENTED_EDGE('',*,*,#1994,.T.);
#2728=ORIENTED_EDGE('',*,*,#1993,.T.);
#2729=ORIENTED_EDGE('',*,*,#1994,.F.);
#2730=ORIENTED_EDGE('',*,*,#1995,.F.);
#2731=ORIENTED_EDGE('',*,*,#1996,.T.);
#2732=ORIENTED_EDGE('',*,*,#1983,.T.);
#2733=ORIENTED_EDGE('',*,*,#1996,.F.);
#2734=ORIENTED_EDGE('',*,*,#1995,.T.);
#2735=ORIENTED_EDGE('',*,*,#1997,.F.);
#2736=ORIENTED_EDGE('',*,*,#1997,.T.);
#2737=ORIENTED_EDGE('',*,*,#1998,.T.);
#2738=ORIENTED_EDGE('',*,*,#1969,.T.);
#2739=ORIENTED_EDGE('',*,*,#1998,.F.);
#2740=ORIENTED_EDGE('',*,*,#1999,.F.);
#2741=ORIENTED_EDGE('',*,*,#2000,.T.);
#2742=ORIENTED_EDGE('',*,*,#2001,.F.);
#2743=ORIENTED_EDGE('',*,*,#2002,.T.);
#2744=ORIENTED_EDGE('',*,*,#1999,.T.);
#2745=ORIENTED_EDGE('',*,*,#2002,.F.);
#2746=ORIENTED_EDGE('',*,*,#2001,.T.);
#2747=ORIENTED_EDGE('',*,*,#2003,.F.);
#2748=ORIENTED_EDGE('',*,*,#2004,.F.);
#2749=ORIENTED_EDGE('',*,*,#2005,.T.);
#2750=ORIENTED_EDGE('',*,*,#2003,.T.);
#2751=ORIENTED_EDGE('',*,*,#2005,.F.);
#2752=ORIENTED_EDGE('',*,*,#2004,.T.);
#2753=ORIENTED_EDGE('',*,*,#2006,.F.);
#2754=ORIENTED_EDGE('',*,*,#2006,.T.);
#2755=ORIENTED_EDGE('',*,*,#2007,.T.);
#2756=ORIENTED_EDGE('',*,*,#2000,.F.);
#2757=ORIENTED_EDGE('',*,*,#2007,.F.);
#2758=ORIENTED_EDGE('',*,*,#2008,.F.);
#2759=ORIENTED_EDGE('',*,*,#2009,.F.);
#2760=ORIENTED_EDGE('',*,*,#2010,.T.);
#2761=ORIENTED_EDGE('',*,*,#2008,.T.);
#2762=ORIENTED_EDGE('',*,*,#2010,.F.);
#2763=ORIENTED_EDGE('',*,*,#2011,.F.);
#2764=ORIENTED_EDGE('',*,*,#2012,.T.);
#2765=ORIENTED_EDGE('',*,*,#2009,.T.);
#2766=ORIENTED_EDGE('',*,*,#2012,.F.);
#2767=ORIENTED_EDGE('',*,*,#2011,.T.);
#2768=ORIENTED_EDGE('',*,*,#2013,.F.);
#2769=ORIENTED_EDGE('',*,*,#2014,.T.);
#2770=ORIENTED_EDGE('',*,*,#2015,.T.);
#2771=ORIENTED_EDGE('',*,*,#2014,.F.);
#2772=ORIENTED_EDGE('',*,*,#2016,.F.);
#2773=ORIENTED_EDGE('',*,*,#2017,.T.);
#2774=ORIENTED_EDGE('',*,*,#2018,.T.);
#2775=ORIENTED_EDGE('',*,*,#2017,.F.);
#2776=ORIENTED_EDGE('',*,*,#2016,.T.);
#2777=ORIENTED_EDGE('',*,*,#2013,.T.);
#2778=ORIENTED_EDGE('',*,*,#2018,.F.);
#2779=ORIENTED_EDGE('',*,*,#2015,.F.);
#2780=ORIENTED_EDGE('',*,*,#2019,.F.);
#2781=ORIENTED_EDGE('',*,*,#2020,.T.);
#2782=ORIENTED_EDGE('',*,*,#2021,.F.);
#2783=ORIENTED_EDGE('',*,*,#2020,.F.);
#2784=ORIENTED_EDGE('',*,*,#2022,.F.);
#2785=ORIENTED_EDGE('',*,*,#2023,.T.);
#2786=ORIENTED_EDGE('',*,*,#2019,.T.);
#2787=ORIENTED_EDGE('',*,*,#2023,.F.);
#2788=ORIENTED_EDGE('',*,*,#2022,.T.);
#2789=ORIENTED_EDGE('',*,*,#2024,.F.);
#2790=ORIENTED_EDGE('',*,*,#2025,.T.);
#2791=ORIENTED_EDGE('',*,*,#2026,.F.);
#2792=ORIENTED_EDGE('',*,*,#2027,.F.);
#2793=ORIENTED_EDGE('',*,*,#2028,.F.);
#2794=ORIENTED_EDGE('',*,*,#2029,.F.);
#2795=ORIENTED_EDGE('',*,*,#2030,.F.);
#2796=ORIENTED_EDGE('',*,*,#2031,.F.);
#2797=ORIENTED_EDGE('',*,*,#2025,.F.);
#2798=ORIENTED_EDGE('',*,*,#2030,.T.);
#2799=ORIENTED_EDGE('',*,*,#2032,.F.);
#2800=ORIENTED_EDGE('',*,*,#2033,.T.);
#2801=ORIENTED_EDGE('',*,*,#2034,.T.);
#2802=ORIENTED_EDGE('',*,*,#2029,.T.);
#2803=ORIENTED_EDGE('',*,*,#2035,.F.);
#2804=ORIENTED_EDGE('',*,*,#2036,.T.);
#2805=ORIENTED_EDGE('',*,*,#2032,.T.);
#2806=ORIENTED_EDGE('',*,*,#2028,.T.);
#2807=ORIENTED_EDGE('',*,*,#2037,.F.);
#2808=ORIENTED_EDGE('',*,*,#2038,.T.);
#2809=ORIENTED_EDGE('',*,*,#2035,.T.);
#2810=ORIENTED_EDGE('',*,*,#2027,.T.);
#2811=ORIENTED_EDGE('',*,*,#2039,.F.);
#2812=ORIENTED_EDGE('',*,*,#2040,.T.);
#2813=ORIENTED_EDGE('',*,*,#2037,.T.);
#2814=ORIENTED_EDGE('',*,*,#2026,.T.);
#2815=ORIENTED_EDGE('',*,*,#2041,.F.);
#2816=ORIENTED_EDGE('',*,*,#2042,.T.);
#2817=ORIENTED_EDGE('',*,*,#2039,.T.);
#2818=ORIENTED_EDGE('',*,*,#2031,.T.);
#2819=ORIENTED_EDGE('',*,*,#2034,.F.);
#2820=ORIENTED_EDGE('',*,*,#2043,.T.);
#2821=ORIENTED_EDGE('',*,*,#2041,.T.);
#2822=ORIENTED_EDGE('',*,*,#2024,.T.);
#2823=ORIENTED_EDGE('',*,*,#2038,.F.);
#2824=ORIENTED_EDGE('',*,*,#2040,.F.);
#2825=ORIENTED_EDGE('',*,*,#2042,.F.);
#2826=ORIENTED_EDGE('',*,*,#2043,.F.);
#2827=ORIENTED_EDGE('',*,*,#2033,.F.);
#2828=ORIENTED_EDGE('',*,*,#2036,.F.);
#2829=ORIENTED_EDGE('',*,*,#2021,.T.);
#2830=PLANE('',#3311);
#2831=PLANE('',#3320);
#2832=PLANE('',#3322);
#2833=PLANE('',#3337);
#2834=PLANE('',#3341);
#2835=PLANE('',#3345);
#2836=PLANE('',#3349);
#2837=PLANE('',#3355);
#2838=PLANE('',#3359);
#2839=PLANE('',#3363);
#2840=PLANE('',#3367);
#2841=PLANE('',#3368);
#2842=PLANE('',#3380);
#2843=PLANE('',#3384);
#2844=PLANE('',#3388);
#2845=PLANE('',#3389);
#2846=PLANE('',#3390);
#2847=PLANE('',#3391);
#2848=PLANE('',#3392);
#2849=PLANE('',#3393);
#2850=PLANE('',#3394);
#2851=PLANE('',#3395);
#2852=PLANE('',#3400);
#2853=PLANE('',#3402);
#2854=PLANE('',#3404);
#2855=PLANE('',#3405);
#2856=PLANE('',#3406);
#2857=PLANE('',#3407);
#2858=PLANE('',#3408);
#2859=PLANE('',#3409);
#2860=PLANE('',#3410);
#2861=PLANE('',#3415);
#2862=PLANE('',#3420);
#2863=PLANE('',#3422);
#2864=PLANE('',#3424);
#2865=PLANE('',#3425);
#2866=PLANE('',#3426);
#2867=PLANE('',#3427);
#2868=PLANE('',#3428);
#2869=PLANE('',#3429);
#2870=PLANE('',#3430);
#2871=PLANE('',#3435);
#2872=PLANE('',#3440);
#2873=PLANE('',#3442);
#2874=PLANE('',#3444);
#2875=PLANE('',#3445);
#2876=PLANE('',#3446);
#2877=PLANE('',#3447);
#2878=PLANE('',#3448);
#2879=PLANE('',#3449);
#2880=PLANE('',#3450);
#2881=PLANE('',#3455);
#2882=PLANE('',#3460);
#2883=PLANE('',#3462);
#2884=PLANE('',#3464);
#2885=PLANE('',#3465);
#2886=PLANE('',#3466);
#2887=PLANE('',#3467);
#2888=PLANE('',#3468);
#2889=PLANE('',#3469);
#2890=PLANE('',#3470);
#2891=PLANE('',#3475);
#2892=PLANE('',#3489);
#2893=PLANE('',#3494);
#2894=PLANE('',#3500);
#2895=PLANE('',#3501);
#2896=PLANE('',#3502);
#2897=PLANE('',#3503);
#2898=PLANE('',#3504);
#2899=PLANE('',#3505);
#2900=PLANE('',#3519);
#2901=PLANE('',#3524);
#2902=PLANE('',#3530);
#2903=PLANE('',#3531);
#2904=PLANE('',#3532);
#2905=PLANE('',#3533);
#2906=PLANE('',#3534);
#2907=PLANE('',#3535);
#2908=PLANE('',#3537);
#2909=PLANE('',#3542);
#2910=PLANE('',#3544);
#2911=PLANE('',#3546);
#2912=PLANE('',#3547);
#2913=PLANE('',#3548);
#2914=PLANE('',#3549);
#2915=PLANE('',#3550);
#2916=PLANE('',#3551);
#2917=PLANE('',#3557);
#2918=PLANE('',#3562);
#2919=PLANE('',#3563);
#2920=PLANE('',#3564);
#2921=PLANE('',#3565);
#2922=PLANE('',#3566);
#2923=PLANE('',#3567);
#2924=PLANE('',#3568);
#2925=PLANE('',#3569);
#2926=PLANE('',#3570);
#2927=PLANE('',#3576);
#2928=PLANE('',#3578);
#2929=PLANE('',#3580);
#2930=PLANE('',#3582);
#2931=PLANE('',#3583);
#2932=PLANE('',#3584);
#2933=PLANE('',#3585);
#2934=PLANE('',#3586);
#2935=PLANE('',#3587);
#2936=PLANE('',#3588);
#2937=PLANE('',#3592);
#2938=PLANE('',#3597);
#2939=PLANE('',#3601);
#2940=PLANE('',#3606);
#2941=PLANE('',#3610);
#2942=PLANE('',#3622);
#2943=PLANE('',#3630);
#2944=PLANE('',#3631);
#2945=PLANE('',#3638);
#2946=PLANE('',#3641);
#2947=PLANE('',#3642);
#2948=PLANE('',#3643);
#2949=PLANE('',#3644);
#2950=PLANE('',#3645);
#2951=PLANE('',#3646);
#2952=PLANE('',#3647);
#2953=PLANE('',#3648);
#2954=ADVANCED_FACE('',(#330),#2830,.T.);
#2955=ADVANCED_FACE('',(#331),#273,.F.);
#2956=ADVANCED_FACE('',(#332),#2831,.T.);
#2957=ADVANCED_FACE('',(#333),#2832,.T.);
#2958=ADVANCED_FACE('',(#334),#274,.F.);
#2959=ADVANCED_FACE('',(#335),#275,.F.);
#2960=ADVANCED_FACE('',(#336),#276,.F.);
#2961=ADVANCED_FACE('',(#337),#2833,.F.);
#2962=ADVANCED_FACE('',(#338),#277,.F.);
#2963=ADVANCED_FACE('',(#339),#2834,.F.);
#2964=ADVANCED_FACE('',(#340),#278,.F.);
#2965=ADVANCED_FACE('',(#341,#178),#2835,.F.);
#2966=ADVANCED_FACE('',(#342),#279,.F.);
#2967=ADVANCED_FACE('',(#343,#179),#2836,.F.);
#2968=ADVANCED_FACE('',(#344),#280,.F.);
#2969=ADVANCED_FACE('',(#345),#281,.F.);
#2970=ADVANCED_FACE('',(#346),#2837,.F.);
#2971=ADVANCED_FACE('',(#347),#282,.F.);
#2972=ADVANCED_FACE('',(#348),#2838,.F.);
#2973=ADVANCED_FACE('',(#349),#283,.F.);
#2974=ADVANCED_FACE('',(#350,#180),#2839,.F.);
#2975=ADVANCED_FACE('',(#351),#284,.F.);
#2976=ADVANCED_FACE('',(#352,#181),#2840,.F.);
#2977=ADVANCED_FACE('',(#353),#2841,.T.);
#2978=ADVANCED_FACE('',(#354,#182,#183),#285,.F.);
#2979=ADVANCED_FACE('',(#355),#2842,.T.);
#2980=ADVANCED_FACE('',(#356),#286,.F.);
#2981=ADVANCED_FACE('',(#357),#2843,.T.);
#2982=ADVANCED_FACE('',(#358),#287,.F.);
#2983=ADVANCED_FACE('',(#359),#2844,.T.);
#2984=ADVANCED_FACE('',(#360),#2845,.T.);
#2985=ADVANCED_FACE('',(#361),#2846,.T.);
#2986=ADVANCED_FACE('',(#362,#184),#2847,.T.);
#2987=ADVANCED_FACE('',(#363),#2848,.T.);
#2988=ADVANCED_FACE('',(#364,#185),#2849,.T.);
#2989=ADVANCED_FACE('',(#365,#186,#187,#188,#189),#2850,.T.);
#2990=ADVANCED_FACE('',(#366,#190,#191,#192,#193,#194,#195),#2851,.F.);
#2991=ADVANCED_FACE('',(#367),#288,.F.);
#2992=ADVANCED_FACE('',(#368,#196),#2852,.T.);
#2993=ADVANCED_FACE('',(#369,#197),#2853,.F.);
#2994=ADVANCED_FACE('',(#370),#2854,.T.);
#2995=ADVANCED_FACE('',(#371),#2855,.T.);
#2996=ADVANCED_FACE('',(#372),#2856,.T.);
#2997=ADVANCED_FACE('',(#373),#2857,.T.);
#2998=ADVANCED_FACE('',(#374),#2858,.T.);
#2999=ADVANCED_FACE('',(#375),#2859,.T.);
#3000=ADVANCED_FACE('',(#376,#198),#2860,.T.);
#3001=ADVANCED_FACE('',(#377),#289,.F.);
#3002=ADVANCED_FACE('',(#378),#290,.T.);
#3003=ADVANCED_FACE('',(#379,#199),#2861,.F.);
#3004=ADVANCED_FACE('',(#380),#291,.F.);
#3005=ADVANCED_FACE('',(#381,#200),#2862,.T.);
#3006=ADVANCED_FACE('',(#382,#201),#2863,.F.);
#3007=ADVANCED_FACE('',(#383),#2864,.T.);
#3008=ADVANCED_FACE('',(#384),#2865,.T.);
#3009=ADVANCED_FACE('',(#385),#2866,.T.);
#3010=ADVANCED_FACE('',(#386),#2867,.T.);
#3011=ADVANCED_FACE('',(#387),#2868,.T.);
#3012=ADVANCED_FACE('',(#388),#2869,.T.);
#3013=ADVANCED_FACE('',(#389,#202),#2870,.T.);
#3014=ADVANCED_FACE('',(#390),#292,.F.);
#3015=ADVANCED_FACE('',(#391),#293,.T.);
#3016=ADVANCED_FACE('',(#392,#203),#2871,.F.);
#3017=ADVANCED_FACE('',(#393),#294,.F.);
#3018=ADVANCED_FACE('',(#394,#204),#2872,.T.);
#3019=ADVANCED_FACE('',(#395,#205),#2873,.F.);
#3020=ADVANCED_FACE('',(#396),#2874,.T.);
#3021=ADVANCED_FACE('',(#397),#2875,.T.);
#3022=ADVANCED_FACE('',(#398),#2876,.T.);
#3023=ADVANCED_FACE('',(#399),#2877,.T.);
#3024=ADVANCED_FACE('',(#400),#2878,.T.);
#3025=ADVANCED_FACE('',(#401),#2879,.T.);
#3026=ADVANCED_FACE('',(#402,#206),#2880,.T.);
#3027=ADVANCED_FACE('',(#403),#295,.F.);
#3028=ADVANCED_FACE('',(#404),#296,.T.);
#3029=ADVANCED_FACE('',(#405,#207),#2881,.F.);
#3030=ADVANCED_FACE('',(#406),#297,.F.);
#3031=ADVANCED_FACE('',(#407,#208),#2882,.T.);
#3032=ADVANCED_FACE('',(#408,#209),#2883,.F.);
#3033=ADVANCED_FACE('',(#409),#2884,.T.);
#3034=ADVANCED_FACE('',(#410),#2885,.T.);
#3035=ADVANCED_FACE('',(#411),#2886,.T.);
#3036=ADVANCED_FACE('',(#412),#2887,.T.);
#3037=ADVANCED_FACE('',(#413),#2888,.T.);
#3038=ADVANCED_FACE('',(#414),#2889,.T.);
#3039=ADVANCED_FACE('',(#415,#210),#2890,.T.);
#3040=ADVANCED_FACE('',(#416),#298,.F.);
#3041=ADVANCED_FACE('',(#417),#299,.T.);
#3042=ADVANCED_FACE('',(#418,#211),#2891,.F.);
#3043=ADVANCED_FACE('',(#419),#300,.F.);
#3044=ADVANCED_FACE('',(#420),#301,.F.);
#3045=ADVANCED_FACE('',(#421),#302,.F.);
#3046=ADVANCED_FACE('',(#422),#303,.F.);
#3047=ADVANCED_FACE('',(#423,#212),#2892,.F.);
#3048=ADVANCED_FACE('',(#424),#304,.F.);
#3049=ADVANCED_FACE('',(#425,#213),#2893,.F.);
#3050=ADVANCED_FACE('',(#426),#305,.F.);
#3051=ADVANCED_FACE('',(#427),#306,.F.);
#3052=ADVANCED_FACE('',(#428),#2894,.T.);
#3053=ADVANCED_FACE('',(#429),#2895,.T.);
#3054=ADVANCED_FACE('',(#430),#2896,.T.);
#3055=ADVANCED_FACE('',(#431),#2897,.T.);
#3056=ADVANCED_FACE('',(#432,#214,#215,#216,#217,#218),#2898,.T.);
#3057=ADVANCED_FACE('',(#433,#219,#220,#221,#222,#223),#2899,.F.);
#3058=ADVANCED_FACE('',(#434),#307,.F.);
#3059=ADVANCED_FACE('',(#435),#308,.F.);
#3060=ADVANCED_FACE('',(#436),#309,.F.);
#3061=ADVANCED_FACE('',(#437),#310,.F.);
#3062=ADVANCED_FACE('',(#438,#224),#2900,.F.);
#3063=ADVANCED_FACE('',(#439),#311,.F.);
#3064=ADVANCED_FACE('',(#440,#225),#2901,.F.);
#3065=ADVANCED_FACE('',(#441),#312,.F.);
#3066=ADVANCED_FACE('',(#442),#313,.F.);
#3067=ADVANCED_FACE('',(#443),#2902,.T.);
#3068=ADVANCED_FACE('',(#444),#2903,.T.);
#3069=ADVANCED_FACE('',(#445),#2904,.T.);
#3070=ADVANCED_FACE('',(#446),#2905,.T.);
#3071=ADVANCED_FACE('',(#447,#226,#227,#228,#229,#230),#2906,.T.);
#3072=ADVANCED_FACE('',(#448,#231,#232,#233,#234,#235),#2907,.F.);
#3073=ADVANCED_FACE('',(#449,#236),#2908,.T.);
#3074=ADVANCED_FACE('',(#450),#314,.F.);
#3075=ADVANCED_FACE('',(#451,#237),#2909,.F.);
#3076=ADVANCED_FACE('',(#452,#238),#2910,.T.);
#3077=ADVANCED_FACE('',(#453),#2911,.T.);
#3078=ADVANCED_FACE('',(#454),#2912,.T.);
#3079=ADVANCED_FACE('',(#455),#2913,.T.);
#3080=ADVANCED_FACE('',(#456),#2914,.T.);
#3081=ADVANCED_FACE('',(#457),#2915,.T.);
#3082=ADVANCED_FACE('',(#458),#2916,.T.);
#3083=ADVANCED_FACE('',(#459),#315,.T.);
#3084=ADVANCED_FACE('',(#460),#316,.T.);
#3085=ADVANCED_FACE('',(#461),#118,.T.);
#3086=ADVANCED_FACE('',(#462,#239),#2917,.T.);
#3087=ADVANCED_FACE('',(#463),#317,.F.);
#3088=ADVANCED_FACE('',(#464),#2918,.F.);
#3089=ADVANCED_FACE('',(#465,#240),#2919,.F.);
#3090=ADVANCED_FACE('',(#466),#2920,.T.);
#3091=ADVANCED_FACE('',(#467),#2921,.T.);
#3092=ADVANCED_FACE('',(#468),#2922,.T.);
#3093=ADVANCED_FACE('',(#469),#2923,.T.);
#3094=ADVANCED_FACE('',(#470),#2924,.T.);
#3095=ADVANCED_FACE('',(#471),#2925,.T.);
#3096=ADVANCED_FACE('',(#472),#2926,.T.);
#3097=ADVANCED_FACE('',(#473),#318,.F.);
#3098=ADVANCED_FACE('',(#474,#241),#2927,.T.);
#3099=ADVANCED_FACE('',(#475,#242),#2928,.T.);
#3100=ADVANCED_FACE('',(#476,#243),#2929,.F.);
#3101=ADVANCED_FACE('',(#477),#2930,.T.);
#3102=ADVANCED_FACE('',(#478),#2931,.T.);
#3103=ADVANCED_FACE('',(#479),#2932,.T.);
#3104=ADVANCED_FACE('',(#480),#2933,.T.);
#3105=ADVANCED_FACE('',(#481),#2934,.T.);
#3106=ADVANCED_FACE('',(#482),#2935,.T.);
#3107=ADVANCED_FACE('',(#483,#244),#2936,.T.);
#3108=ADVANCED_FACE('',(#484),#319,.F.);
#3109=ADVANCED_FACE('',(#485,#245),#2937,.T.);
#3110=ADVANCED_FACE('',(#486),#320,.T.);
#3111=ADVANCED_FACE('',(#487),#321,.T.);
#3112=ADVANCED_FACE('',(#488,#246),#2938,.T.);
#3113=ADVANCED_FACE('',(#489),#322,.F.);
#3114=ADVANCED_FACE('',(#490,#247),#2939,.T.);
#3115=ADVANCED_FACE('',(#491),#323,.T.);
#3116=ADVANCED_FACE('',(#492,#248),#2940,.T.);
#3117=ADVANCED_FACE('',(#493),#324,.T.);
#3118=ADVANCED_FACE('',(#494,#249),#2941,.T.);
#3119=ADVANCED_FACE('',(#495),#325,.F.);
#3120=ADVANCED_FACE('',(#496),#17,.T.);
#3121=ADVANCED_FACE('',(#497),#326,.T.);
#3122=ADVANCED_FACE('',(#498),#119,.T.);
#3123=ADVANCED_FACE('',(#499),#2942,.T.);
#3124=ADVANCED_FACE('',(#500),#327,.F.);
#3125=ADVANCED_FACE('',(#501),#328,.T.);
#3126=ADVANCED_FACE('',(#502,#250),#2943,.T.);
#3127=ADVANCED_FACE('',(#503,#251),#2944,.F.);
#3128=ADVANCED_FACE('',(#504),#329,.T.);
#3129=ADVANCED_FACE('',(#505),#120,.T.);
#3130=ADVANCED_FACE('',(#506),#2945,.T.);
#3131=ADVANCED_FACE('',(#507),#121,.T.);
#3132=ADVANCED_FACE('',(#508),#2946,.T.);
#3133=ADVANCED_FACE('',(#509),#2947,.T.);
#3134=ADVANCED_FACE('',(#510),#2948,.T.);
#3135=ADVANCED_FACE('',(#511),#2949,.T.);
#3136=ADVANCED_FACE('',(#512),#2950,.T.);
#3137=ADVANCED_FACE('',(#513),#2951,.T.);
#3138=ADVANCED_FACE('',(#514),#2952,.T.);
#3139=ADVANCED_FACE('',(#515,#252),#2953,.F.);
#3140=CLOSED_SHELL('',(#2954,#2955,#2956,#2957,#2958,#2959,#2960,#2961,
#2962,#2963,#2964,#2965,#2966,#2967,#2968,#2969,#2970,#2971,#2972,#2973,
#2974,#2975,#2976,#2977,#2978,#2979,#2980,#2981,#2982,#2983,#2984,#2985,
#2986,#2987,#2988,#2989,#2990));
#3141=CLOSED_SHELL('',(#2991,#2992,#2993,#2994,#2995,#2996,#2997,#2998,
#2999,#3000,#3001,#3002,#3003));
#3142=CLOSED_SHELL('',(#3004,#3005,#3006,#3007,#3008,#3009,#3010,#3011,
#3012,#3013,#3014,#3015,#3016));
#3143=CLOSED_SHELL('',(#3017,#3018,#3019,#3020,#3021,#3022,#3023,#3024,
#3025,#3026,#3027,#3028,#3029));
#3144=CLOSED_SHELL('',(#3030,#3031,#3032,#3033,#3034,#3035,#3036,#3037,
#3038,#3039,#3040,#3041,#3042));
#3145=CLOSED_SHELL('',(#3043,#3044,#3045,#3046,#3047,#3048,#3049,#3050,
#3051,#3052,#3053,#3054,#3055,#3056,#3057));
#3146=CLOSED_SHELL('',(#3058,#3059,#3060,#3061,#3062,#3063,#3064,#3065,
#3066,#3067,#3068,#3069,#3070,#3071,#3072));
#3147=CLOSED_SHELL('',(#3073,#3074,#3075,#3076,#3077,#3078,#3079,#3080,
#3081,#3082,#3083,#3084,#3085,#3086));
#3148=CLOSED_SHELL('',(#3087,#3088,#3089,#3090,#3091,#3092,#3093,#3094,
#3095,#3096));
#3149=CLOSED_SHELL('',(#3097,#3098,#3099,#3100,#3101,#3102,#3103,#3104,
#3105,#3106,#3107,#3108,#3109,#3110,#3111,#3112,#3113));
#3150=CLOSED_SHELL('',(#3114,#3115,#3116,#3117,#3118,#3119));
#3151=CLOSED_SHELL('',(#3120,#3121,#3122,#3123));
#3152=CLOSED_SHELL('',(#3124,#3125,#3126,#3127));
#3153=CLOSED_SHELL('',(#3128,#3129,#3130,#3131,#3132,#3133,#3134,#3135,
#3136,#3137,#3138,#3139));
#3154=DERIVED_UNIT_ELEMENT(#3182,1.);
#3155=DERIVED_UNIT_ELEMENT(#5640,-3.);
#3156=DERIVED_UNIT_ELEMENT(#3182,1.);
#3157=DERIVED_UNIT_ELEMENT(#5640,-3.);
#3158=DERIVED_UNIT_ELEMENT(#3182,1.);
#3159=DERIVED_UNIT_ELEMENT(#5640,-3.);
#3160=DERIVED_UNIT_ELEMENT(#3182,1.);
#3161=DERIVED_UNIT_ELEMENT(#5640,-3.);
#3162=DERIVED_UNIT_ELEMENT(#3182,1.);
#3163=DERIVED_UNIT_ELEMENT(#5640,-3.);
#3164=DERIVED_UNIT_ELEMENT(#3182,1.);
#3165=DERIVED_UNIT_ELEMENT(#5640,-3.);
#3166=DERIVED_UNIT_ELEMENT(#3182,1.);
#3167=DERIVED_UNIT_ELEMENT(#5640,-3.);
#3168=DERIVED_UNIT_ELEMENT(#3182,1.);
#3169=DERIVED_UNIT_ELEMENT(#5640,-3.);
#3170=DERIVED_UNIT_ELEMENT(#3182,1.);
#3171=DERIVED_UNIT_ELEMENT(#5640,-3.);
#3172=DERIVED_UNIT_ELEMENT(#3182,1.);
#3173=DERIVED_UNIT_ELEMENT(#5640,-3.);
#3174=DERIVED_UNIT_ELEMENT(#3182,1.);
#3175=DERIVED_UNIT_ELEMENT(#5640,-3.);
#3176=DERIVED_UNIT_ELEMENT(#3182,1.);
#3177=DERIVED_UNIT_ELEMENT(#5640,-3.);
#3178=DERIVED_UNIT_ELEMENT(#3182,1.);
#3179=DERIVED_UNIT_ELEMENT(#5640,-3.);
#3180=DERIVED_UNIT_ELEMENT(#3182,1.);
#3181=DERIVED_UNIT_ELEMENT(#5640,-3.);
#3182=(
MASS_UNIT()
NAMED_UNIT(*)
SI_UNIT(.KILO.,.GRAM.)
);
#3183=DERIVED_UNIT((#3154,#3155));
#3184=DERIVED_UNIT((#3156,#3157));
#3185=DERIVED_UNIT((#3158,#3159));
#3186=DERIVED_UNIT((#3160,#3161));
#3187=DERIVED_UNIT((#3162,#3163));
#3188=DERIVED_UNIT((#3164,#3165));
#3189=DERIVED_UNIT((#3166,#3167));
#3190=DERIVED_UNIT((#3168,#3169));
#3191=DERIVED_UNIT((#3170,#3171));
#3192=DERIVED_UNIT((#3172,#3173));
#3193=DERIVED_UNIT((#3174,#3175));
#3194=DERIVED_UNIT((#3176,#3177));
#3195=DERIVED_UNIT((#3178,#3179));
#3196=DERIVED_UNIT((#3180,#3181));
#3197=MEASURE_REPRESENTATION_ITEM('density measure',
POSITIVE_RATIO_MEASURE(7850.),#3183);
#3198=MEASURE_REPRESENTATION_ITEM('density measure',
POSITIVE_RATIO_MEASURE(7850.),#3184);
#3199=MEASURE_REPRESENTATION_ITEM('density measure',
POSITIVE_RATIO_MEASURE(7850.),#3185);
#3200=MEASURE_REPRESENTATION_ITEM('density measure',
POSITIVE_RATIO_MEASURE(7850.),#3186);
#3201=MEASURE_REPRESENTATION_ITEM('density measure',
POSITIVE_RATIO_MEASURE(7850.),#3187);
#3202=MEASURE_REPRESENTATION_ITEM('density measure',
POSITIVE_RATIO_MEASURE(7850.),#3188);
#3203=MEASURE_REPRESENTATION_ITEM('density measure',
POSITIVE_RATIO_MEASURE(7850.),#3189);
#3204=MEASURE_REPRESENTATION_ITEM('density measure',
POSITIVE_RATIO_MEASURE(7850.),#3190);
#3205=MEASURE_REPRESENTATION_ITEM('density measure',
POSITIVE_RATIO_MEASURE(7850.),#3191);
#3206=MEASURE_REPRESENTATION_ITEM('density measure',
POSITIVE_RATIO_MEASURE(7850.),#3192);
#3207=MEASURE_REPRESENTATION_ITEM('density measure',
POSITIVE_RATIO_MEASURE(7850.),#3193);
#3208=MEASURE_REPRESENTATION_ITEM('density measure',
POSITIVE_RATIO_MEASURE(7850.),#3194);
#3209=MEASURE_REPRESENTATION_ITEM('density measure',
POSITIVE_RATIO_MEASURE(7850.),#3195);
#3210=MEASURE_REPRESENTATION_ITEM('density measure',
POSITIVE_RATIO_MEASURE(7850.),#3196);
#3211=PROPERTY_DEFINITION_REPRESENTATION(#3281,#3239);
#3212=PROPERTY_DEFINITION_REPRESENTATION(#3282,#3240);
#3213=PROPERTY_DEFINITION_REPRESENTATION(#3283,#3241);
#3214=PROPERTY_DEFINITION_REPRESENTATION(#3284,#3242);
#3215=PROPERTY_DEFINITION_REPRESENTATION(#3285,#3243);
#3216=PROPERTY_DEFINITION_REPRESENTATION(#3286,#3244);
#3217=PROPERTY_DEFINITION_REPRESENTATION(#3287,#3245);
#3218=PROPERTY_DEFINITION_REPRESENTATION(#3288,#3246);
#3219=PROPERTY_DEFINITION_REPRESENTATION(#3289,#3247);
#3220=PROPERTY_DEFINITION_REPRESENTATION(#3290,#3248);
#3221=PROPERTY_DEFINITION_REPRESENTATION(#3291,#3249);
#3222=PROPERTY_DEFINITION_REPRESENTATION(#3292,#3250);
#3223=PROPERTY_DEFINITION_REPRESENTATION(#3293,#3251);
#3224=PROPERTY_DEFINITION_REPRESENTATION(#3294,#3252);
#3225=PROPERTY_DEFINITION_REPRESENTATION(#3295,#3253);
#3226=PROPERTY_DEFINITION_REPRESENTATION(#3296,#3254);
#3227=PROPERTY_DEFINITION_REPRESENTATION(#3297,#3255);
#3228=PROPERTY_DEFINITION_REPRESENTATION(#3298,#3256);
#3229=PROPERTY_DEFINITION_REPRESENTATION(#3299,#3257);
#3230=PROPERTY_DEFINITION_REPRESENTATION(#3300,#3258);
#3231=PROPERTY_DEFINITION_REPRESENTATION(#3301,#3259);
#3232=PROPERTY_DEFINITION_REPRESENTATION(#3302,#3260);
#3233=PROPERTY_DEFINITION_REPRESENTATION(#3303,#3261);
#3234=PROPERTY_DEFINITION_REPRESENTATION(#3304,#3262);
#3235=PROPERTY_DEFINITION_REPRESENTATION(#3305,#3263);
#3236=PROPERTY_DEFINITION_REPRESENTATION(#3306,#3264);
#3237=PROPERTY_DEFINITION_REPRESENTATION(#3307,#3265);
#3238=PROPERTY_DEFINITION_REPRESENTATION(#3308,#3266);
#3239=REPRESENTATION('material name',(#3267),#5623);
#3240=REPRESENTATION('density',(#3197),#5623);
#3241=REPRESENTATION('material name',(#3268),#5624);
#3242=REPRESENTATION('density',(#3198),#5624);
#3243=REPRESENTATION('material name',(#3269),#5625);
#3244=REPRESENTATION('density',(#3199),#5625);
#3245=REPRESENTATION('material name',(#3270),#5626);
#3246=REPRESENTATION('density',(#3200),#5626);
#3247=REPRESENTATION('material name',(#3271),#5627);
#3248=REPRESENTATION('density',(#3201),#5627);
#3249=REPRESENTATION('material name',(#3272),#5628);
#3250=REPRESENTATION('density',(#3202),#5628);
#3251=REPRESENTATION('material name',(#3273),#5629);
#3252=REPRESENTATION('density',(#3203),#5629);
#3253=REPRESENTATION('material name',(#3274),#5630);
#3254=REPRESENTATION('density',(#3204),#5630);
#3255=REPRESENTATION('material name',(#3275),#5631);
#3256=REPRESENTATION('density',(#3205),#5631);
#3257=REPRESENTATION('material name',(#3276),#5633);
#3258=REPRESENTATION('density',(#3206),#5633);
#3259=REPRESENTATION('material name',(#3277),#5634);
#3260=REPRESENTATION('density',(#3207),#5634);
#3261=REPRESENTATION('material name',(#3278),#5635);
#3262=REPRESENTATION('density',(#3208),#5635);
#3263=REPRESENTATION('material name',(#3279),#5636);
#3264=REPRESENTATION('density',(#3209),#5636);
#3265=REPRESENTATION('material name',(#3280),#5637);
#3266=REPRESENTATION('density',(#3210),#5637);
#3267=DESCRIPTIVE_REPRESENTATION_ITEM('Steel','Steel');
#3268=DESCRIPTIVE_REPRESENTATION_ITEM('Steel','Steel');
#3269=DESCRIPTIVE_REPRESENTATION_ITEM('Steel','Steel');
#3270=DESCRIPTIVE_REPRESENTATION_ITEM('Steel','Steel');
#3271=DESCRIPTIVE_REPRESENTATION_ITEM('Steel','Steel');
#3272=DESCRIPTIVE_REPRESENTATION_ITEM('Steel','Steel');
#3273=DESCRIPTIVE_REPRESENTATION_ITEM('Steel','Steel');
#3274=DESCRIPTIVE_REPRESENTATION_ITEM('Steel','Steel');
#3275=DESCRIPTIVE_REPRESENTATION_ITEM('Steel','Steel');
#3276=DESCRIPTIVE_REPRESENTATION_ITEM('Steel','Steel');
#3277=DESCRIPTIVE_REPRESENTATION_ITEM('Steel','Steel');
#3278=DESCRIPTIVE_REPRESENTATION_ITEM('Steel','Steel');
#3279=DESCRIPTIVE_REPRESENTATION_ITEM('Steel','Steel');
#3280=DESCRIPTIVE_REPRESENTATION_ITEM('Steel','Steel');
#3281=PROPERTY_DEFINITION('material property','material name',#5718);
#3282=PROPERTY_DEFINITION('material property','density of part',#5718);
#3283=PROPERTY_DEFINITION('material property','material name',#5719);
#3284=PROPERTY_DEFINITION('material property','density of part',#5719);
#3285=PROPERTY_DEFINITION('material property','material name',#5720);
#3286=PROPERTY_DEFINITION('material property','density of part',#5720);
#3287=PROPERTY_DEFINITION('material property','material name',#5721);
#3288=PROPERTY_DEFINITION('material property','density of part',#5721);
#3289=PROPERTY_DEFINITION('material property','material name',#5722);
#3290=PROPERTY_DEFINITION('material property','density of part',#5722);
#3291=PROPERTY_DEFINITION('material property','material name',#5723);
#3292=PROPERTY_DEFINITION('material property','density of part',#5723);
#3293=PROPERTY_DEFINITION('material property','material name',#5724);
#3294=PROPERTY_DEFINITION('material property','density of part',#5724);
#3295=PROPERTY_DEFINITION('material property','material name',#5725);
#3296=PROPERTY_DEFINITION('material property','density of part',#5725);
#3297=PROPERTY_DEFINITION('material property','material name',#5726);
#3298=PROPERTY_DEFINITION('material property','density of part',#5726);
#3299=PROPERTY_DEFINITION('material property','material name',#5728);
#3300=PROPERTY_DEFINITION('material property','density of part',#5728);
#3301=PROPERTY_DEFINITION('material property','material name',#5729);
#3302=PROPERTY_DEFINITION('material property','density of part',#5729);
#3303=PROPERTY_DEFINITION('material property','material name',#5730);
#3304=PROPERTY_DEFINITION('material property','density of part',#5730);
#3305=PROPERTY_DEFINITION('material property','material name',#5731);
#3306=PROPERTY_DEFINITION('material property','density of part',#5731);
#3307=PROPERTY_DEFINITION('material property','material name',#5732);
#3308=PROPERTY_DEFINITION('material property','density of part',#5732);
#3309=AXIS2_PLACEMENT_3D('',#4645,#3672,#3673);
#3310=AXIS2_PLACEMENT_3D('',#4646,#3674,#3675);
#3311=AXIS2_PLACEMENT_3D('',#4647,#3676,#3677);
#3312=AXIS2_PLACEMENT_3D('',#4651,#3679,#3680);
#3313=AXIS2_PLACEMENT_3D('',#4652,#3681,#3682);
#3314=AXIS2_PLACEMENT_3D('',#4655,#3683,#3684);
#3315=AXIS2_PLACEMENT_3D('',#4656,#3685,#3686);
#3316=AXIS2_PLACEMENT_3D('',#4658,#3687,#3688);
#3317=AXIS2_PLACEMENT_3D('',#4661,#3690,#3691);
#3318=AXIS2_PLACEMENT_3D('',#4663,#3692,#3693);
#3319=AXIS2_PLACEMENT_3D('',#4664,#3694,#3695);
#3320=AXIS2_PLACEMENT_3D('',#4665,#3696,#3697);
#3321=AXIS2_PLACEMENT_3D('',#4669,#3699,#3700);
#3322=AXIS2_PLACEMENT_3D('',#4670,#3701,#3702);
#3323=AXIS2_PLACEMENT_3D('',#4674,#3704,#3705);
#3324=AXIS2_PLACEMENT_3D('',#4675,#3706,#3707);
#3325=AXIS2_PLACEMENT_3D('',#4678,#3708,#3709);
#3326=AXIS2_PLACEMENT_3D('',#4681,#3711,#3712);
#3327=AXIS2_PLACEMENT_3D('',#4683,#3713,#3714);
#3328=AXIS2_PLACEMENT_3D('',#4685,#3715,#3716);
#3329=AXIS2_PLACEMENT_3D('',#4687,#3717,#3718);
#3330=AXIS2_PLACEMENT_3D('',#4689,#3719,#3720);
#3331=AXIS2_PLACEMENT_3D('',#4690,#3721,#3722);
#3332=AXIS2_PLACEMENT_3D('',#4691,#3723,#3724);
#3333=AXIS2_PLACEMENT_3D('',#4693,#3725,#3726);
#3334=AXIS2_PLACEMENT_3D('',#4733,#3728,#3729);
#3335=AXIS2_PLACEMENT_3D('',#4735,#3730,#3731);
#3336=AXIS2_PLACEMENT_3D('',#4738,#3733,#3734);
#3337=AXIS2_PLACEMENT_3D('',#4739,#3735,#3736);
#3338=AXIS2_PLACEMENT_3D('',#4740,#3737,#3738);
#3339=AXIS2_PLACEMENT_3D('',#4742,#3739,#3740);
#3340=AXIS2_PLACEMENT_3D('',#4745,#3742,#3743);
#3341=AXIS2_PLACEMENT_3D('',#4746,#3744,#3745);
#3342=AXIS2_PLACEMENT_3D('',#4747,#3746,#3747);
#3343=AXIS2_PLACEMENT_3D('',#4749,#3748,#3749);
#3344=AXIS2_PLACEMENT_3D('',#4752,#3751,#3752);
#3345=AXIS2_PLACEMENT_3D('',#4753,#3753,#3754);
#3346=AXIS2_PLACEMENT_3D('',#4754,#3755,#3756);
#3347=AXIS2_PLACEMENT_3D('',#4756,#3757,#3758);
#3348=AXIS2_PLACEMENT_3D('',#4759,#3760,#3761);
#3349=AXIS2_PLACEMENT_3D('',#4760,#3762,#3763);
#3350=AXIS2_PLACEMENT_3D('',#4761,#3764,#3765);
#3351=AXIS2_PLACEMENT_3D('',#4763,#3766,#3767);
#3352=AXIS2_PLACEMENT_3D('',#4803,#3769,#3770);
#3353=AXIS2_PLACEMENT_3D('',#4805,#3771,#3772);
#3354=AXIS2_PLACEMENT_3D('',#4808,#3774,#3775);
#3355=AXIS2_PLACEMENT_3D('',#4809,#3776,#3777);
#3356=AXIS2_PLACEMENT_3D('',#4810,#3778,#3779);
#3357=AXIS2_PLACEMENT_3D('',#4812,#3780,#3781);
#3358=AXIS2_PLACEMENT_3D('',#4815,#3783,#3784);
#3359=AXIS2_PLACEMENT_3D('',#4816,#3785,#3786);
#3360=AXIS2_PLACEMENT_3D('',#4817,#3787,#3788);
#3361=AXIS2_PLACEMENT_3D('',#4819,#3789,#3790);
#3362=AXIS2_PLACEMENT_3D('',#4822,#3792,#3793);
#3363=AXIS2_PLACEMENT_3D('',#4823,#3794,#3795);
#3364=AXIS2_PLACEMENT_3D('',#4824,#3796,#3797);
#3365=AXIS2_PLACEMENT_3D('',#4826,#3798,#3799);
#3366=AXIS2_PLACEMENT_3D('',#4829,#3801,#3802);
#3367=AXIS2_PLACEMENT_3D('',#4830,#3803,#3804);
#3368=AXIS2_PLACEMENT_3D('',#4831,#3805,#3806);
#3369=AXIS2_PLACEMENT_3D('',#4833,#3808,#3809);
#3370=AXIS2_PLACEMENT_3D('',#4835,#3810,#3811);
#3371=AXIS2_PLACEMENT_3D('',#4841,#3815,#3816);
#3372=AXIS2_PLACEMENT_3D('',#4845,#3818,#3819);
#3373=AXIS2_PLACEMENT_3D('',#4849,#3821,#3822);
#3374=AXIS2_PLACEMENT_3D('',#4853,#3824,#3825);
#3375=AXIS2_PLACEMENT_3D('',#4857,#3828,#3829);
#3376=AXIS2_PLACEMENT_3D('',#4858,#3830,#3831);
#3377=AXIS2_PLACEMENT_3D('',#4859,#3832,#3833);
#3378=AXIS2_PLACEMENT_3D('',#4860,#3834,#3835);
#3379=AXIS2_PLACEMENT_3D('',#4861,#3836,#3837);
#3380=AXIS2_PLACEMENT_3D('',#4863,#3839,#3840);
#3381=AXIS2_PLACEMENT_3D('',#4864,#3841,#3842);
#3382=AXIS2_PLACEMENT_3D('',#4865,#3843,#3844);
#3383=AXIS2_PLACEMENT_3D('',#4868,#3846,#3847);
#3384=AXIS2_PLACEMENT_3D('',#4869,#3848,#3849);
#3385=AXIS2_PLACEMENT_3D('',#4870,#3850,#3851);
#3386=AXIS2_PLACEMENT_3D('',#4871,#3852,#3853);
#3387=AXIS2_PLACEMENT_3D('',#4874,#3855,#3856);
#3388=AXIS2_PLACEMENT_3D('',#4875,#3857,#3858);
#3389=AXIS2_PLACEMENT_3D('',#4876,#3859,#3860);
#3390=AXIS2_PLACEMENT_3D('',#4877,#3861,#3862);
#3391=AXIS2_PLACEMENT_3D('',#4886,#3867,#3868);
#3392=AXIS2_PLACEMENT_3D('',#4892,#3872,#3873);
#3393=AXIS2_PLACEMENT_3D('',#4898,#3877,#3878);
#3394=AXIS2_PLACEMENT_3D('',#4901,#3881,#3882);
#3395=AXIS2_PLACEMENT_3D('',#4902,#3883,#3884);
#3396=AXIS2_PLACEMENT_3D('',#4903,#3885,#3886);
#3397=AXIS2_PLACEMENT_3D('',#4904,#3887,#3888);
#3398=AXIS2_PLACEMENT_3D('',#4906,#3889,#3890);
#3399=AXIS2_PLACEMENT_3D('',#4909,#3892,#3893);
#3400=AXIS2_PLACEMENT_3D('',#4910,#3894,#3895);
#3401=AXIS2_PLACEMENT_3D('',#4912,#3896,#3897);
#3402=AXIS2_PLACEMENT_3D('',#4913,#3898,#3899);
#3403=AXIS2_PLACEMENT_3D('',#4927,#3906,#3907);
#3404=AXIS2_PLACEMENT_3D('',#4928,#3908,#3909);
#3405=AXIS2_PLACEMENT_3D('',#4934,#3913,#3914);
#3406=AXIS2_PLACEMENT_3D('',#4938,#3917,#3918);
#3407=AXIS2_PLACEMENT_3D('',#4942,#3921,#3922);
#3408=AXIS2_PLACEMENT_3D('',#4946,#3925,#3926);
#3409=AXIS2_PLACEMENT_3D('',#4950,#3929,#3930);
#3410=AXIS2_PLACEMENT_3D('',#4952,#3932,#3933);
#3411=AXIS2_PLACEMENT_3D('',#4953,#3934,#3935);
#3412=AXIS2_PLACEMENT_3D('',#4956,#3937,#3938);
#3413=AXIS2_PLACEMENT_3D('',#4957,#3939,#3940);
#3414=AXIS2_PLACEMENT_3D('',#4960,#3942,#3943);
#3415=AXIS2_PLACEMENT_3D('',#4961,#3944,#3945);
#3416=AXIS2_PLACEMENT_3D('',#4962,#3946,#3947);
#3417=AXIS2_PLACEMENT_3D('',#4963,#3948,#3949);
#3418=AXIS2_PLACEMENT_3D('',#4965,#3950,#3951);
#3419=AXIS2_PLACEMENT_3D('',#4968,#3953,#3954);
#3420=AXIS2_PLACEMENT_3D('',#4969,#3955,#3956);
#3421=AXIS2_PLACEMENT_3D('',#4971,#3957,#3958);
#3422=AXIS2_PLACEMENT_3D('',#4972,#3959,#3960);
#3423=AXIS2_PLACEMENT_3D('',#4986,#3967,#3968);
#3424=AXIS2_PLACEMENT_3D('',#4987,#3969,#3970);
#3425=AXIS2_PLACEMENT_3D('',#4993,#3974,#3975);
#3426=AXIS2_PLACEMENT_3D('',#4997,#3978,#3979);
#3427=AXIS2_PLACEMENT_3D('',#5001,#3982,#3983);
#3428=AXIS2_PLACEMENT_3D('',#5005,#3986,#3987);
#3429=AXIS2_PLACEMENT_3D('',#5009,#3990,#3991);
#3430=AXIS2_PLACEMENT_3D('',#5011,#3993,#3994);
#3431=AXIS2_PLACEMENT_3D('',#5012,#3995,#3996);
#3432=AXIS2_PLACEMENT_3D('',#5015,#3998,#3999);
#3433=AXIS2_PLACEMENT_3D('',#5016,#4000,#4001);
#3434=AXIS2_PLACEMENT_3D('',#5019,#4003,#4004);
#3435=AXIS2_PLACEMENT_3D('',#5020,#4005,#4006);
#3436=AXIS2_PLACEMENT_3D('',#5021,#4007,#4008);
#3437=AXIS2_PLACEMENT_3D('',#5022,#4009,#4010);
#3438=AXIS2_PLACEMENT_3D('',#5024,#4011,#4012);
#3439=AXIS2_PLACEMENT_3D('',#5027,#4014,#4015);
#3440=AXIS2_PLACEMENT_3D('',#5028,#4016,#4017);
#3441=AXIS2_PLACEMENT_3D('',#5030,#4018,#4019);
#3442=AXIS2_PLACEMENT_3D('',#5031,#4020,#4021);
#3443=AXIS2_PLACEMENT_3D('',#5045,#4028,#4029);
#3444=AXIS2_PLACEMENT_3D('',#5046,#4030,#4031);
#3445=AXIS2_PLACEMENT_3D('',#5052,#4035,#4036);
#3446=AXIS2_PLACEMENT_3D('',#5056,#4039,#4040);
#3447=AXIS2_PLACEMENT_3D('',#5060,#4043,#4044);
#3448=AXIS2_PLACEMENT_3D('',#5064,#4047,#4048);
#3449=AXIS2_PLACEMENT_3D('',#5068,#4051,#4052);
#3450=AXIS2_PLACEMENT_3D('',#5070,#4054,#4055);
#3451=AXIS2_PLACEMENT_3D('',#5071,#4056,#4057);
#3452=AXIS2_PLACEMENT_3D('',#5074,#4059,#4060);
#3453=AXIS2_PLACEMENT_3D('',#5075,#4061,#4062);
#3454=AXIS2_PLACEMENT_3D('',#5078,#4064,#4065);
#3455=AXIS2_PLACEMENT_3D('',#5079,#4066,#4067);
#3456=AXIS2_PLACEMENT_3D('',#5080,#4068,#4069);
#3457=AXIS2_PLACEMENT_3D('',#5081,#4070,#4071);
#3458=AXIS2_PLACEMENT_3D('',#5083,#4072,#4073);
#3459=AXIS2_PLACEMENT_3D('',#5086,#4075,#4076);
#3460=AXIS2_PLACEMENT_3D('',#5087,#4077,#4078);
#3461=AXIS2_PLACEMENT_3D('',#5089,#4079,#4080);
#3462=AXIS2_PLACEMENT_3D('',#5090,#4081,#4082);
#3463=AXIS2_PLACEMENT_3D('',#5104,#4089,#4090);
#3464=AXIS2_PLACEMENT_3D('',#5105,#4091,#4092);
#3465=AXIS2_PLACEMENT_3D('',#5111,#4096,#4097);
#3466=AXIS2_PLACEMENT_3D('',#5115,#4100,#4101);
#3467=AXIS2_PLACEMENT_3D('',#5119,#4104,#4105);
#3468=AXIS2_PLACEMENT_3D('',#5123,#4108,#4109);
#3469=AXIS2_PLACEMENT_3D('',#5127,#4112,#4113);
#3470=AXIS2_PLACEMENT_3D('',#5129,#4115,#4116);
#3471=AXIS2_PLACEMENT_3D('',#5130,#4117,#4118);
#3472=AXIS2_PLACEMENT_3D('',#5133,#4120,#4121);
#3473=AXIS2_PLACEMENT_3D('',#5134,#4122,#4123);
#3474=AXIS2_PLACEMENT_3D('',#5137,#4125,#4126);
#3475=AXIS2_PLACEMENT_3D('',#5138,#4127,#4128);
#3476=AXIS2_PLACEMENT_3D('',#5139,#4129,#4130);
#3477=AXIS2_PLACEMENT_3D('',#5140,#4131,#4132);
#3478=AXIS2_PLACEMENT_3D('',#5142,#4133,#4134);
#3479=AXIS2_PLACEMENT_3D('',#5145,#4136,#4137);
#3480=AXIS2_PLACEMENT_3D('',#5146,#4138,#4139);
#3481=AXIS2_PLACEMENT_3D('',#5148,#4140,#4141);
#3482=AXIS2_PLACEMENT_3D('',#5151,#4143,#4144);
#3483=AXIS2_PLACEMENT_3D('',#5152,#4145,#4146);
#3484=AXIS2_PLACEMENT_3D('',#5154,#4147,#4148);
#3485=AXIS2_PLACEMENT_3D('',#5157,#4150,#4151);
#3486=AXIS2_PLACEMENT_3D('',#5158,#4152,#4153);
#3487=AXIS2_PLACEMENT_3D('',#5160,#4154,#4155);
#3488=AXIS2_PLACEMENT_3D('',#5163,#4157,#4158);
#3489=AXIS2_PLACEMENT_3D('',#5164,#4159,#4160);
#3490=AXIS2_PLACEMENT_3D('',#5166,#4161,#4162);
#3491=AXIS2_PLACEMENT_3D('',#5167,#4163,#4164);
#3492=AXIS2_PLACEMENT_3D('',#5169,#4165,#4166);
#3493=AXIS2_PLACEMENT_3D('',#5172,#4168,#4169);
#3494=AXIS2_PLACEMENT_3D('',#5173,#4170,#4171);
#3495=AXIS2_PLACEMENT_3D('',#5175,#4172,#4173);
#3496=AXIS2_PLACEMENT_3D('',#5176,#4174,#4175);
#3497=AXIS2_PLACEMENT_3D('',#5179,#4177,#4178);
#3498=AXIS2_PLACEMENT_3D('',#5180,#4179,#4180);
#3499=AXIS2_PLACEMENT_3D('',#5183,#4182,#4183);
#3500=AXIS2_PLACEMENT_3D('',#5184,#4184,#4185);
#3501=AXIS2_PLACEMENT_3D('',#5193,#4190,#4191);
#3502=AXIS2_PLACEMENT_3D('',#5199,#4195,#4196);
#3503=AXIS2_PLACEMENT_3D('',#5205,#4200,#4201);
#3504=AXIS2_PLACEMENT_3D('',#5208,#4204,#4205);
#3505=AXIS2_PLACEMENT_3D('',#5209,#4206,#4207);
#3506=AXIS2_PLACEMENT_3D('',#5210,#4208,#4209);
#3507=AXIS2_PLACEMENT_3D('',#5211,#4210,#4211);
#3508=AXIS2_PLACEMENT_3D('',#5213,#4212,#4213);
#3509=AXIS2_PLACEMENT_3D('',#5216,#4215,#4216);
#3510=AXIS2_PLACEMENT_3D('',#5217,#4217,#4218);
#3511=AXIS2_PLACEMENT_3D('',#5219,#4219,#4220);
#3512=AXIS2_PLACEMENT_3D('',#5222,#4222,#4223);
#3513=AXIS2_PLACEMENT_3D('',#5223,#4224,#4225);
#3514=AXIS2_PLACEMENT_3D('',#5225,#4226,#4227);
#3515=AXIS2_PLACEMENT_3D('',#5228,#4229,#4230);
#3516=AXIS2_PLACEMENT_3D('',#5229,#4231,#4232);
#3517=AXIS2_PLACEMENT_3D('',#5231,#4233,#4234);
#3518=AXIS2_PLACEMENT_3D('',#5234,#4236,#4237);
#3519=AXIS2_PLACEMENT_3D('',#5235,#4238,#4239);
#3520=AXIS2_PLACEMENT_3D('',#5237,#4240,#4241);
#3521=AXIS2_PLACEMENT_3D('',#5238,#4242,#4243);
#3522=AXIS2_PLACEMENT_3D('',#5240,#4244,#4245);
#3523=AXIS2_PLACEMENT_3D('',#5243,#4247,#4248);
#3524=AXIS2_PLACEMENT_3D('',#5244,#4249,#4250);
#3525=AXIS2_PLACEMENT_3D('',#5246,#4251,#4252);
#3526=AXIS2_PLACEMENT_3D('',#5247,#4253,#4254);
#3527=AXIS2_PLACEMENT_3D('',#5250,#4256,#4257);
#3528=AXIS2_PLACEMENT_3D('',#5251,#4258,#4259);
#3529=AXIS2_PLACEMENT_3D('',#5254,#4261,#4262);
#3530=AXIS2_PLACEMENT_3D('',#5255,#4263,#4264);
#3531=AXIS2_PLACEMENT_3D('',#5264,#4269,#4270);
#3532=AXIS2_PLACEMENT_3D('',#5270,#4274,#4275);
#3533=AXIS2_PLACEMENT_3D('',#5276,#4279,#4280);
#3534=AXIS2_PLACEMENT_3D('',#5279,#4283,#4284);
#3535=AXIS2_PLACEMENT_3D('',#5280,#4285,#4286);
#3536=AXIS2_PLACEMENT_3D('',#5281,#4287,#4288);
#3537=AXIS2_PLACEMENT_3D('',#5282,#4289,#4290);
#3538=AXIS2_PLACEMENT_3D('',#5284,#4291,#4292);
#3539=AXIS2_PLACEMENT_3D('',#5286,#4293,#4294);
#3540=AXIS2_PLACEMENT_3D('',#5287,#4295,#4296);
#3541=AXIS2_PLACEMENT_3D('',#5289,#4297,#4298);
#3542=AXIS2_PLACEMENT_3D('',#5291,#4300,#4301);
#3543=AXIS2_PLACEMENT_3D('',#5305,#4308,#4309);
#3544=AXIS2_PLACEMENT_3D('',#5306,#4310,#4311);
#3545=AXIS2_PLACEMENT_3D('',#5320,#4318,#4319);
#3546=AXIS2_PLACEMENT_3D('',#5321,#4320,#4321);
#3547=AXIS2_PLACEMENT_3D('',#5324,#4324,#4325);
#3548=AXIS2_PLACEMENT_3D('',#5326,#4327,#4328);
#3549=AXIS2_PLACEMENT_3D('',#5328,#4330,#4331);
#3550=AXIS2_PLACEMENT_3D('',#5330,#4333,#4334);
#3551=AXIS2_PLACEMENT_3D('',#5332,#4336,#4337);
#3552=AXIS2_PLACEMENT_3D('',#5333,#4338,#4339);
#3553=AXIS2_PLACEMENT_3D('',#5335,#4341,#4342);
#3554=AXIS2_PLACEMENT_3D('',#5337,#4343,#4344);
#3555=AXIS2_PLACEMENT_3D('',#5339,#4346,#4347);
#3556=AXIS2_PLACEMENT_3D('',#5341,#4348,#4349);
#3557=AXIS2_PLACEMENT_3D('',#5343,#4351,#4352);
#3558=AXIS2_PLACEMENT_3D('',#5344,#4353,#4354);
#3559=AXIS2_PLACEMENT_3D('',#5345,#4355,#4356);
#3560=AXIS2_PLACEMENT_3D('',#5347,#4357,#4358);
#3561=AXIS2_PLACEMENT_3D('',#5350,#4360,#4361);
#3562=AXIS2_PLACEMENT_3D('',#5351,#4362,#4363);
#3563=AXIS2_PLACEMENT_3D('',#5352,#4364,#4365);
#3564=AXIS2_PLACEMENT_3D('',#5365,#4372,#4373);
#3565=AXIS2_PLACEMENT_3D('',#5371,#4377,#4378);
#3566=AXIS2_PLACEMENT_3D('',#5375,#4381,#4382);
#3567=AXIS2_PLACEMENT_3D('',#5379,#4385,#4386);
#3568=AXIS2_PLACEMENT_3D('',#5383,#4389,#4390);
#3569=AXIS2_PLACEMENT_3D('',#5387,#4393,#4394);
#3570=AXIS2_PLACEMENT_3D('',#5389,#4396,#4397);
#3571=AXIS2_PLACEMENT_3D('',#5390,#4398,#4399);
#3572=AXIS2_PLACEMENT_3D('',#5391,#4400,#4401);
#3573=AXIS2_PLACEMENT_3D('',#5392,#4402,#4403);
#3574=AXIS2_PLACEMENT_3D('',#5394,#4404,#4405);
#3575=AXIS2_PLACEMENT_3D('',#5397,#4407,#4408);
#3576=AXIS2_PLACEMENT_3D('',#5398,#4409,#4410);
#3577=AXIS2_PLACEMENT_3D('',#5400,#4411,#4412);
#3578=AXIS2_PLACEMENT_3D('',#5401,#4413,#4414);
#3579=AXIS2_PLACEMENT_3D('',#5415,#4421,#4422);
#3580=AXIS2_PLACEMENT_3D('',#5416,#4423,#4424);
#3581=AXIS2_PLACEMENT_3D('',#5430,#4431,#4432);
#3582=AXIS2_PLACEMENT_3D('',#5431,#4433,#4434);
#3583=AXIS2_PLACEMENT_3D('',#5434,#4437,#4438);
#3584=AXIS2_PLACEMENT_3D('',#5436,#4440,#4441);
#3585=AXIS2_PLACEMENT_3D('',#5438,#4443,#4444);
#3586=AXIS2_PLACEMENT_3D('',#5440,#4446,#4447);
#3587=AXIS2_PLACEMENT_3D('',#5442,#4449,#4450);
#3588=AXIS2_PLACEMENT_3D('',#5443,#4451,#4452);
#3589=AXIS2_PLACEMENT_3D('',#5445,#4453,#4454);
#3590=AXIS2_PLACEMENT_3D('',#5446,#4455,#4456);
#3591=AXIS2_PLACEMENT_3D('',#5449,#4458,#4459);
#3592=AXIS2_PLACEMENT_3D('',#5450,#4460,#4461);
#3593=AXIS2_PLACEMENT_3D('',#5452,#4462,#4463);
#3594=AXIS2_PLACEMENT_3D('',#5453,#4464,#4465);
#3595=AXIS2_PLACEMENT_3D('',#5455,#4467,#4468);
#3596=AXIS2_PLACEMENT_3D('',#5457,#4469,#4470);
#3597=AXIS2_PLACEMENT_3D('',#5459,#4472,#4473);
#3598=AXIS2_PLACEMENT_3D('',#5461,#4474,#4475);
#3599=AXIS2_PLACEMENT_3D('',#5462,#4476,#4477);
#3600=AXIS2_PLACEMENT_3D('',#5464,#4479,#4480);
#3601=AXIS2_PLACEMENT_3D('',#5465,#4481,#4482);
#3602=AXIS2_PLACEMENT_3D('',#5467,#4483,#4484);
#3603=AXIS2_PLACEMENT_3D('',#5469,#4485,#4486);
#3604=AXIS2_PLACEMENT_3D('',#5470,#4487,#4488);
#3605=AXIS2_PLACEMENT_3D('',#5472,#4489,#4490);
#3606=AXIS2_PLACEMENT_3D('',#5474,#4492,#4493);
#3607=AXIS2_PLACEMENT_3D('',#5476,#4494,#4495);
#3608=AXIS2_PLACEMENT_3D('',#5477,#4496,#4497);
#3609=AXIS2_PLACEMENT_3D('',#5479,#4498,#4499);
#3610=AXIS2_PLACEMENT_3D('',#5481,#4501,#4502);
#3611=AXIS2_PLACEMENT_3D('',#5483,#4503,#4504);
#3612=AXIS2_PLACEMENT_3D('',#5484,#4505,#4506);
#3613=AXIS2_PLACEMENT_3D('',#5486,#4508,#4509);
#3614=AXIS2_PLACEMENT_3D('',#5487,#4510,#4511);
#3615=AXIS2_PLACEMENT_3D('',#5488,#4512,#4513);
#3616=AXIS2_PLACEMENT_3D('',#5489,#4514,#4515);
#3617=AXIS2_PLACEMENT_3D('',#5491,#4516,#4517);
#3618=AXIS2_PLACEMENT_3D('',#5492,#4518,#4519);
#3619=AXIS2_PLACEMENT_3D('',#5494,#4520,#4521);
#3620=AXIS2_PLACEMENT_3D('',#5496,#4523,#4524);
#3621=AXIS2_PLACEMENT_3D('',#5498,#4525,#4526);
#3622=AXIS2_PLACEMENT_3D('',#5500,#4528,#4529);
#3623=AXIS2_PLACEMENT_3D('',#5501,#4530,#4531);
#3624=AXIS2_PLACEMENT_3D('',#5502,#4532,#4533);
#3625=AXIS2_PLACEMENT_3D('',#5504,#4534,#4535);
#3626=AXIS2_PLACEMENT_3D('',#5507,#4537,#4538);
#3627=AXIS2_PLACEMENT_3D('',#5508,#4539,#4540);
#3628=AXIS2_PLACEMENT_3D('',#5510,#4541,#4542);
#3629=AXIS2_PLACEMENT_3D('',#5513,#4544,#4545);
#3630=AXIS2_PLACEMENT_3D('',#5514,#4546,#4547);
#3631=AXIS2_PLACEMENT_3D('',#5515,#4548,#4549);
#3632=AXIS2_PLACEMENT_3D('',#5516,#4550,#4551);
#3633=AXIS2_PLACEMENT_3D('',#5517,#4552,#4553);
#3634=AXIS2_PLACEMENT_3D('',#5519,#4554,#4555);
#3635=AXIS2_PLACEMENT_3D('',#5522,#4557,#4558);
#3636=AXIS2_PLACEMENT_3D('',#5523,#4559,#4560);
#3637=AXIS2_PLACEMENT_3D('',#5525,#4561,#4562);
#3638=AXIS2_PLACEMENT_3D('',#5527,#4564,#4565);
#3639=AXIS2_PLACEMENT_3D('',#5528,#4566,#4567);
#3640=AXIS2_PLACEMENT_3D('',#5530,#4568,#4569);
#3641=AXIS2_PLACEMENT_3D('',#5556,#4571,#4572);
#3642=AXIS2_PLACEMENT_3D('',#5562,#4576,#4577);
#3643=AXIS2_PLACEMENT_3D('',#5566,#4580,#4581);
#3644=AXIS2_PLACEMENT_3D('',#5570,#4584,#4585);
#3645=AXIS2_PLACEMENT_3D('',#5574,#4588,#4589);
#3646=AXIS2_PLACEMENT_3D('',#5578,#4592,#4593);
#3647=AXIS2_PLACEMENT_3D('',#5580,#4595,#4596);
#3648=AXIS2_PLACEMENT_3D('',#5581,#4597,#4598);
#3649=AXIS2_PLACEMENT_3D('',#5582,#4599,#4600);
#3650=AXIS2_PLACEMENT_3D('',#5583,#4601,#4602);
#3651=AXIS2_PLACEMENT_3D('',#5584,#4603,#4604);
#3652=AXIS2_PLACEMENT_3D('',#5585,#4605,#4606);
#3653=AXIS2_PLACEMENT_3D('',#5586,#4607,#4608);
#3654=AXIS2_PLACEMENT_3D('',#5587,#4609,#4610);
#3655=AXIS2_PLACEMENT_3D('',#5588,#4611,#4612);
#3656=AXIS2_PLACEMENT_3D('',#5589,#4613,#4614);
#3657=AXIS2_PLACEMENT_3D('',#5590,#4615,#4616);
#3658=AXIS2_PLACEMENT_3D('',#5591,#4617,#4618);
#3659=AXIS2_PLACEMENT_3D('',#5592,#4619,#4620);
#3660=AXIS2_PLACEMENT_3D('',#5593,#4621,#4622);
#3661=AXIS2_PLACEMENT_3D('',#5594,#4623,#4624);
#3662=AXIS2_PLACEMENT_3D('',#5595,#4625,#4626);
#3663=AXIS2_PLACEMENT_3D('',#5596,#4627,#4628);
#3664=AXIS2_PLACEMENT_3D('',#5597,#4629,#4630);
#3665=AXIS2_PLACEMENT_3D('',#5598,#4631,#4632);
#3666=AXIS2_PLACEMENT_3D('',#5599,#4633,#4634);
#3667=AXIS2_PLACEMENT_3D('',#5600,#4635,#4636);
#3668=AXIS2_PLACEMENT_3D('',#5601,#4637,#4638);
#3669=AXIS2_PLACEMENT_3D('',#5602,#4639,#4640);
#3670=AXIS2_PLACEMENT_3D('',#5603,#4641,#4642);
#3671=AXIS2_PLACEMENT_3D('',#5604,#4643,#4644);
#3672=DIRECTION('axis',(0.,0.,1.));
#3673=DIRECTION('refdir',(1.,0.,0.));
#3674=DIRECTION('axis',(0.,0.,1.));
#3675=DIRECTION('refdir',(1.,0.,0.));
#3676=DIRECTION('center_axis',(0.,0.,1.));
#3677=DIRECTION('ref_axis',(1.,0.,0.));
#3678=DIRECTION('',(-1.,0.,0.));
#3679=DIRECTION('center_axis',(0.,0.,1.));
#3680=DIRECTION('ref_axis',(1.,0.,0.));
#3681=DIRECTION('center_axis',(0.,0.,1.));
#3682=DIRECTION('ref_axis',(1.,0.,0.));
#3683=DIRECTION('center_axis',(0.707106781186548,0.,-0.707106781186547));
#3684=DIRECTION('ref_axis',(-0.707106781186547,0.,-0.707106781186548));
#3685=DIRECTION('center_axis',(0.707106781186548,0.,-0.707106781186547));
#3686=DIRECTION('ref_axis',(-0.707106781186547,0.,-0.707106781186548));
#3687=DIRECTION('center_axis',(-0.707106781186548,0.,-0.707106781186547));
#3688=DIRECTION('ref_axis',(0.707106781186547,0.,-0.707106781186548));
#3689=DIRECTION('',(0.,0.,1.));
#3690=DIRECTION('center_axis',(0.,0.,-1.));
#3691=DIRECTION('ref_axis',(1.,0.,0.));
#3692=DIRECTION('center_axis',(-0.707106781186548,0.,-0.707106781186547));
#3693=DIRECTION('ref_axis',(0.707106781186547,0.,-0.707106781186548));
#3694=DIRECTION('center_axis',(0.,0.,1.));
#3695=DIRECTION('ref_axis',(1.,0.,0.));
#3696=DIRECTION('center_axis',(0.,0.,1.));
#3697=DIRECTION('ref_axis',(1.,0.,0.));
#3698=DIRECTION('',(1.,0.,0.));
#3699=DIRECTION('center_axis',(0.,0.,1.));
#3700=DIRECTION('ref_axis',(1.,0.,0.));
#3701=DIRECTION('center_axis',(0.,0.,1.));
#3702=DIRECTION('ref_axis',(1.,0.,0.));
#3703=DIRECTION('',(1.,0.,0.));
#3704=DIRECTION('center_axis',(0.,0.,1.));
#3705=DIRECTION('ref_axis',(1.,0.,0.));
#3706=DIRECTION('center_axis',(0.,0.,1.));
#3707=DIRECTION('ref_axis',(1.,0.,0.));
#3708=DIRECTION('center_axis',(-0.707106781186548,0.,-0.707106781186548));
#3709=DIRECTION('ref_axis',(0.707106781186548,0.,-0.707106781186548));
#3710=DIRECTION('',(0.,0.,1.));
#3711=DIRECTION('center_axis',(0.,0.,-1.));
#3712=DIRECTION('ref_axis',(1.,0.,0.));
#3713=DIRECTION('center_axis',(-0.707106781186548,0.,-0.707106781186548));
#3714=DIRECTION('ref_axis',(0.707106781186548,0.,-0.707106781186548));
#3715=DIRECTION('center_axis',(0.,0.,1.));
#3716=DIRECTION('ref_axis',(1.,0.,0.));
#3717=DIRECTION('center_axis',(0.707106781186548,0.,-0.707106781186547));
#3718=DIRECTION('ref_axis',(-0.707106781186547,0.,-0.707106781186548));
#3719=DIRECTION('center_axis',(0.707106781186548,0.,-0.707106781186547));
#3720=DIRECTION('ref_axis',(-0.707106781186547,0.,-0.707106781186548));
#3721=DIRECTION('center_axis',(0.,0.,1.));
#3722=DIRECTION('ref_axis',(1.,0.,0.));
#3723=DIRECTION('center_axis',(0.,0.,1.));
#3724=DIRECTION('ref_axis',(1.,0.,0.));
#3725=DIRECTION('center_axis',(0.,0.,1.));
#3726=DIRECTION('ref_axis',(1.,0.,0.));
#3727=DIRECTION('',(0.,0.,1.));
#3728=DIRECTION('center_axis',(0.,0.,1.));
#3729=DIRECTION('ref_axis',(1.,0.,0.));
#3730=DIRECTION('center_axis',(0.,0.,1.));
#3731=DIRECTION('ref_axis',(1.,0.,0.));
#3732=DIRECTION('',(0.,0.,1.));
#3733=DIRECTION('center_axis',(0.,0.,1.));
#3734=DIRECTION('ref_axis',(1.,0.,0.));
#3735=DIRECTION('center_axis',(0.,0.,1.));
#3736=DIRECTION('ref_axis',(1.,0.,0.));
#3737=DIRECTION('center_axis',(0.,0.,1.));
#3738=DIRECTION('ref_axis',(1.,0.,0.));
#3739=DIRECTION('center_axis',(0.,0.,1.));
#3740=DIRECTION('ref_axis',(1.,0.,0.));
#3741=DIRECTION('',(0.,0.,1.));
#3742=DIRECTION('center_axis',(0.,0.,1.));
#3743=DIRECTION('ref_axis',(1.,0.,0.));
#3744=DIRECTION('center_axis',(0.,0.,1.));
#3745=DIRECTION('ref_axis',(1.,0.,0.));
#3746=DIRECTION('center_axis',(0.,0.,1.));
#3747=DIRECTION('ref_axis',(1.,0.,0.));
#3748=DIRECTION('center_axis',(0.,0.,1.));
#3749=DIRECTION('ref_axis',(1.,0.,0.));
#3750=DIRECTION('',(0.,0.,1.));
#3751=DIRECTION('center_axis',(0.,0.,1.));
#3752=DIRECTION('ref_axis',(1.,0.,0.));
#3753=DIRECTION('center_axis',(0.,0.,1.));
#3754=DIRECTION('ref_axis',(1.,0.,0.));
#3755=DIRECTION('center_axis',(0.,0.,1.));
#3756=DIRECTION('ref_axis',(1.,0.,0.));
#3757=DIRECTION('center_axis',(0.,0.,1.));
#3758=DIRECTION('ref_axis',(1.,0.,0.));
#3759=DIRECTION('',(0.,0.,1.));
#3760=DIRECTION('center_axis',(0.,0.,1.));
#3761=DIRECTION('ref_axis',(1.,0.,0.));
#3762=DIRECTION('center_axis',(0.,0.,1.));
#3763=DIRECTION('ref_axis',(1.,0.,0.));
#3764=DIRECTION('center_axis',(0.,0.,1.));
#3765=DIRECTION('ref_axis',(1.,0.,0.));
#3766=DIRECTION('center_axis',(0.,0.,1.));
#3767=DIRECTION('ref_axis',(1.,0.,0.));
#3768=DIRECTION('',(0.,0.,1.));
#3769=DIRECTION('center_axis',(0.,0.,1.));
#3770=DIRECTION('ref_axis',(1.,0.,0.));
#3771=DIRECTION('center_axis',(0.,0.,1.));
#3772=DIRECTION('ref_axis',(1.,0.,0.));
#3773=DIRECTION('',(0.,0.,1.));
#3774=DIRECTION('center_axis',(0.,0.,1.));
#3775=DIRECTION('ref_axis',(1.,0.,0.));
#3776=DIRECTION('center_axis',(0.,0.,1.));
#3777=DIRECTION('ref_axis',(1.,0.,0.));
#3778=DIRECTION('center_axis',(0.,0.,1.));
#3779=DIRECTION('ref_axis',(1.,0.,0.));
#3780=DIRECTION('center_axis',(0.,0.,1.));
#3781=DIRECTION('ref_axis',(1.,0.,0.));
#3782=DIRECTION('',(0.,0.,1.));
#3783=DIRECTION('center_axis',(0.,0.,1.));
#3784=DIRECTION('ref_axis',(1.,0.,0.));
#3785=DIRECTION('center_axis',(0.,0.,1.));
#3786=DIRECTION('ref_axis',(1.,0.,0.));
#3787=DIRECTION('center_axis',(0.,0.,1.));
#3788=DIRECTION('ref_axis',(1.,0.,0.));
#3789=DIRECTION('center_axis',(0.,0.,1.));
#3790=DIRECTION('ref_axis',(1.,0.,0.));
#3791=DIRECTION('',(0.,0.,1.));
#3792=DIRECTION('center_axis',(0.,0.,1.));
#3793=DIRECTION('ref_axis',(1.,0.,0.));
#3794=DIRECTION('center_axis',(0.,0.,1.));
#3795=DIRECTION('ref_axis',(1.,0.,0.));
#3796=DIRECTION('center_axis',(0.,0.,1.));
#3797=DIRECTION('ref_axis',(1.,0.,0.));
#3798=DIRECTION('center_axis',(0.,0.,1.));
#3799=DIRECTION('ref_axis',(1.,0.,0.));
#3800=DIRECTION('',(0.,0.,1.));
#3801=DIRECTION('center_axis',(0.,0.,1.));
#3802=DIRECTION('ref_axis',(1.,0.,0.));
#3803=DIRECTION('center_axis',(0.,0.,1.));
#3804=DIRECTION('ref_axis',(1.,0.,0.));
#3805=DIRECTION('center_axis',(0.,0.,1.));
#3806=DIRECTION('ref_axis',(1.,0.,0.));
#3807=DIRECTION('',(1.,0.,0.));
#3808=DIRECTION('center_axis',(1.,0.,0.));
#3809=DIRECTION('ref_axis',(0.,0.,-1.));
#3810=DIRECTION('center_axis',(1.,0.,0.));
#3811=DIRECTION('ref_axis',(0.,0.,-1.));
#3812=DIRECTION('',(1.,0.,0.));
#3813=DIRECTION('',(-1.,0.,0.));
#3814=DIRECTION('',(1.,0.,0.));
#3815=DIRECTION('center_axis',(-0.707106781186548,0.,-0.707106781186547));
#3816=DIRECTION('ref_axis',(0.707106781186547,0.,-0.707106781186548));
#3817=DIRECTION('',(-1.,0.,0.));
#3818=DIRECTION('center_axis',(0.707106781186548,0.,-0.707106781186547));
#3819=DIRECTION('ref_axis',(-0.707106781186547,0.,-0.707106781186548));
#3820=DIRECTION('',(1.,0.,0.));
#3821=DIRECTION('center_axis',(-0.707106781186548,0.,-0.707106781186547));
#3822=DIRECTION('ref_axis',(0.707106781186547,0.,-0.707106781186548));
#3823=DIRECTION('',(-1.,0.,0.));
#3824=DIRECTION('center_axis',(0.707106781186548,0.,-0.707106781186547));
#3825=DIRECTION('ref_axis',(-0.707106781186547,0.,-0.707106781186548));
#3826=DIRECTION('',(1.,0.,0.));
#3827=DIRECTION('',(1.,0.,0.));
#3828=DIRECTION('center_axis',(-1.,0.,0.));
#3829=DIRECTION('ref_axis',(0.,0.,-1.));
#3830=DIRECTION('center_axis',(0.707106781186548,0.,-0.707106781186547));
#3831=DIRECTION('ref_axis',(-0.707106781186547,0.,-0.707106781186548));
#3832=DIRECTION('center_axis',(-0.707106781186548,0.,-0.707106781186547));
#3833=DIRECTION('ref_axis',(0.707106781186547,0.,-0.707106781186548));
#3834=DIRECTION('center_axis',(0.707106781186548,0.,-0.707106781186547));
#3835=DIRECTION('ref_axis',(-0.707106781186547,0.,-0.707106781186548));
#3836=DIRECTION('center_axis',(-0.707106781186548,0.,-0.707106781186547));
#3837=DIRECTION('ref_axis',(0.707106781186547,0.,-0.707106781186548));
#3838=DIRECTION('',(1.,0.,0.));
#3839=DIRECTION('center_axis',(0.,0.,1.));
#3840=DIRECTION('ref_axis',(1.,0.,0.));
#3841=DIRECTION('center_axis',(0.,0.,1.));
#3842=DIRECTION('ref_axis',(1.,0.,0.));
#3843=DIRECTION('center_axis',(0.,0.,1.));
#3844=DIRECTION('ref_axis',(1.,0.,0.));
#3845=DIRECTION('',(0.,0.,1.));
#3846=DIRECTION('center_axis',(0.,0.,-1.));
#3847=DIRECTION('ref_axis',(1.,0.,0.));
#3848=DIRECTION('center_axis',(0.,0.,1.));
#3849=DIRECTION('ref_axis',(1.,0.,0.));
#3850=DIRECTION('center_axis',(0.,0.,1.));
#3851=DIRECTION('ref_axis',(1.,0.,0.));
#3852=DIRECTION('center_axis',(0.,0.,1.));
#3853=DIRECTION('ref_axis',(1.,0.,0.));
#3854=DIRECTION('',(0.,0.,1.));
#3855=DIRECTION('center_axis',(0.,0.,-1.));
#3856=DIRECTION('ref_axis',(1.,0.,0.));
#3857=DIRECTION('center_axis',(0.,0.,1.));
#3858=DIRECTION('ref_axis',(1.,0.,0.));
#3859=DIRECTION('center_axis',(0.,0.,1.));
#3860=DIRECTION('ref_axis',(1.,0.,0.));
#3861=DIRECTION('center_axis',(0.,1.,0.));
#3862=DIRECTION('ref_axis',(-1.,0.,0.));
#3863=DIRECTION('',(-1.,0.,0.));
#3864=DIRECTION('',(0.,0.,1.));
#3865=DIRECTION('',(-1.,0.,0.));
#3866=DIRECTION('',(0.,0.,1.));
#3867=DIRECTION('center_axis',(1.,0.,0.));
#3868=DIRECTION('ref_axis',(0.,1.,0.));
#3869=DIRECTION('',(0.,1.,0.));
#3870=DIRECTION('',(0.,1.,0.));
#3871=DIRECTION('',(0.,0.,1.));
#3872=DIRECTION('center_axis',(0.,-1.,0.));
#3873=DIRECTION('ref_axis',(1.,0.,0.));
#3874=DIRECTION('',(1.,0.,0.));
#3875=DIRECTION('',(1.,0.,0.));
#3876=DIRECTION('',(0.,0.,1.));
#3877=DIRECTION('center_axis',(-1.,0.,0.));
#3878=DIRECTION('ref_axis',(0.,-1.,0.));
#3879=DIRECTION('',(0.,-1.,0.));
#3880=DIRECTION('',(0.,-1.,0.));
#3881=DIRECTION('center_axis',(0.,0.,1.));
#3882=DIRECTION('ref_axis',(1.,0.,0.));
#3883=DIRECTION('center_axis',(0.,0.,1.));
#3884=DIRECTION('ref_axis',(1.,0.,0.));
#3885=DIRECTION('axis',(0.,0.,1.));
#3886=DIRECTION('refdir',(1.,0.,0.));
#3887=DIRECTION('center_axis',(0.,0.,1.));
#3888=DIRECTION('ref_axis',(1.,0.,0.));
#3889=DIRECTION('center_axis',(0.,0.,1.));
#3890=DIRECTION('ref_axis',(1.,0.,0.));
#3891=DIRECTION('',(0.,0.,1.));
#3892=DIRECTION('center_axis',(0.,0.,-1.));
#3893=DIRECTION('ref_axis',(1.,0.,0.));
#3894=DIRECTION('center_axis',(0.,0.,1.));
#3895=DIRECTION('ref_axis',(1.,0.,0.));
#3896=DIRECTION('center_axis',(0.,0.,1.));
#3897=DIRECTION('ref_axis',(1.,0.,0.));
#3898=DIRECTION('center_axis',(0.,0.,1.));
#3899=DIRECTION('ref_axis',(1.,0.,0.));
#3900=DIRECTION('',(0.5,0.866025403784438,0.));
#3901=DIRECTION('',(1.,-3.29650746237182E-16,0.));
#3902=DIRECTION('',(0.499999999999999,-0.866025403784439,0.));
#3903=DIRECTION('',(-0.5,-0.866025403784439,0.));
#3904=DIRECTION('',(-1.,0.,0.));
#3905=DIRECTION('',(-0.5,0.866025403784438,0.));
#3906=DIRECTION('center_axis',(0.,0.,1.));
#3907=DIRECTION('ref_axis',(1.,0.,0.));
#3908=DIRECTION('center_axis',(-3.29650746237182E-16,-1.,0.));
#3909=DIRECTION('ref_axis',(1.,-3.29650746237182E-16,0.));
#3910=DIRECTION('',(0.,0.,1.));
#3911=DIRECTION('',(1.,-3.29650746237182E-16,0.));
#3912=DIRECTION('',(0.,0.,1.));
#3913=DIRECTION('center_axis',(-0.866025403784439,-0.499999999999999,0.));
#3914=DIRECTION('ref_axis',(0.499999999999999,-0.866025403784439,0.));
#3915=DIRECTION('',(0.499999999999999,-0.866025403784439,0.));
#3916=DIRECTION('',(0.,0.,1.));
#3917=DIRECTION('center_axis',(-0.866025403784439,0.5,0.));
#3918=DIRECTION('ref_axis',(-0.5,-0.866025403784439,0.));
#3919=DIRECTION('',(-0.5,-0.866025403784439,0.));
#3920=DIRECTION('',(0.,0.,1.));
#3921=DIRECTION('center_axis',(0.,1.,0.));
#3922=DIRECTION('ref_axis',(-1.,0.,0.));
#3923=DIRECTION('',(-1.,0.,0.));
#3924=DIRECTION('',(0.,0.,1.));
#3925=DIRECTION('center_axis',(0.866025403784438,0.5,0.));
#3926=DIRECTION('ref_axis',(-0.5,0.866025403784438,0.));
#3927=DIRECTION('',(-0.5,0.866025403784438,0.));
#3928=DIRECTION('',(0.,0.,1.));
#3929=DIRECTION('center_axis',(0.866025403784438,-0.5,0.));
#3930=DIRECTION('ref_axis',(0.5,0.866025403784438,0.));
#3931=DIRECTION('',(0.5,0.866025403784438,0.));
#3932=DIRECTION('center_axis',(0.,0.,1.));
#3933=DIRECTION('ref_axis',(1.,0.,0.));
#3934=DIRECTION('center_axis',(0.,0.,1.));
#3935=DIRECTION('ref_axis',(1.,0.,0.));
#3936=DIRECTION('',(0.,0.,-1.));
#3937=DIRECTION('center_axis',(0.,0.,-1.));
#3938=DIRECTION('ref_axis',(1.,0.,0.));
#3939=DIRECTION('center_axis',(0.,0.,1.));
#3940=DIRECTION('ref_axis',(1.,0.,0.));
#3941=DIRECTION('',(0.,0.,-1.));
#3942=DIRECTION('center_axis',(0.,0.,1.));
#3943=DIRECTION('ref_axis',(1.,0.,0.));
#3944=DIRECTION('center_axis',(0.,0.,1.));
#3945=DIRECTION('ref_axis',(1.,0.,0.));
#3946=DIRECTION('axis',(0.,0.,1.));
#3947=DIRECTION('refdir',(1.,0.,0.));
#3948=DIRECTION('center_axis',(0.,0.,1.));
#3949=DIRECTION('ref_axis',(1.,0.,0.));
#3950=DIRECTION('center_axis',(0.,0.,1.));
#3951=DIRECTION('ref_axis',(1.,0.,0.));
#3952=DIRECTION('',(0.,0.,1.));
#3953=DIRECTION('center_axis',(0.,0.,-1.));
#3954=DIRECTION('ref_axis',(1.,0.,0.));
#3955=DIRECTION('center_axis',(0.,0.,1.));
#3956=DIRECTION('ref_axis',(1.,0.,0.));
#3957=DIRECTION('center_axis',(0.,0.,1.));
#3958=DIRECTION('ref_axis',(1.,0.,0.));
#3959=DIRECTION('center_axis',(0.,0.,1.));
#3960=DIRECTION('ref_axis',(1.,0.,0.));
#3961=DIRECTION('',(0.5,0.866025403784439,0.));
#3962=DIRECTION('',(1.,-3.29650746237182E-16,0.));
#3963=DIRECTION('',(0.5,-0.866025403784439,0.));
#3964=DIRECTION('',(-0.500000000000001,-0.866025403784438,0.));
#3965=DIRECTION('',(-1.,0.,0.));
#3966=DIRECTION('',(-0.5,0.866025403784439,0.));
#3967=DIRECTION('center_axis',(0.,0.,1.));
#3968=DIRECTION('ref_axis',(1.,0.,0.));
#3969=DIRECTION('center_axis',(-3.29650746237182E-16,-1.,0.));
#3970=DIRECTION('ref_axis',(1.,-3.29650746237182E-16,0.));
#3971=DIRECTION('',(0.,0.,1.));
#3972=DIRECTION('',(1.,-3.29650746237182E-16,0.));
#3973=DIRECTION('',(0.,0.,1.));
#3974=DIRECTION('center_axis',(-0.866025403784439,-0.5,0.));
#3975=DIRECTION('ref_axis',(0.5,-0.866025403784439,0.));
#3976=DIRECTION('',(0.5,-0.866025403784439,0.));
#3977=DIRECTION('',(0.,0.,1.));
#3978=DIRECTION('center_axis',(-0.866025403784438,0.500000000000001,0.));
#3979=DIRECTION('ref_axis',(-0.500000000000001,-0.866025403784438,0.));
#3980=DIRECTION('',(-0.500000000000001,-0.866025403784438,0.));
#3981=DIRECTION('',(0.,0.,1.));
#3982=DIRECTION('center_axis',(0.,1.,0.));
#3983=DIRECTION('ref_axis',(-1.,0.,0.));
#3984=DIRECTION('',(-1.,0.,0.));
#3985=DIRECTION('',(0.,0.,1.));
#3986=DIRECTION('center_axis',(0.866025403784439,0.5,0.));
#3987=DIRECTION('ref_axis',(-0.5,0.866025403784439,0.));
#3988=DIRECTION('',(-0.5,0.866025403784439,0.));
#3989=DIRECTION('',(0.,0.,1.));
#3990=DIRECTION('center_axis',(0.866025403784439,-0.5,0.));
#3991=DIRECTION('ref_axis',(0.5,0.866025403784439,0.));
#3992=DIRECTION('',(0.5,0.866025403784439,0.));
#3993=DIRECTION('center_axis',(0.,0.,1.));
#3994=DIRECTION('ref_axis',(1.,0.,0.));
#3995=DIRECTION('center_axis',(0.,0.,1.));
#3996=DIRECTION('ref_axis',(1.,0.,0.));
#3997=DIRECTION('',(0.,0.,-1.));
#3998=DIRECTION('center_axis',(0.,0.,-1.));
#3999=DIRECTION('ref_axis',(1.,0.,0.));
#4000=DIRECTION('center_axis',(0.,0.,1.));
#4001=DIRECTION('ref_axis',(1.,0.,0.));
#4002=DIRECTION('',(0.,0.,-1.));
#4003=DIRECTION('center_axis',(0.,0.,1.));
#4004=DIRECTION('ref_axis',(1.,0.,0.));
#4005=DIRECTION('center_axis',(0.,0.,1.));
#4006=DIRECTION('ref_axis',(1.,0.,0.));
#4007=DIRECTION('axis',(0.,0.,1.));
#4008=DIRECTION('refdir',(1.,0.,0.));
#4009=DIRECTION('center_axis',(0.,0.,1.));
#4010=DIRECTION('ref_axis',(1.,0.,0.));
#4011=DIRECTION('center_axis',(0.,0.,1.));
#4012=DIRECTION('ref_axis',(1.,0.,0.));
#4013=DIRECTION('',(0.,0.,1.));
#4014=DIRECTION('center_axis',(0.,0.,-1.));
#4015=DIRECTION('ref_axis',(1.,0.,0.));
#4016=DIRECTION('center_axis',(0.,0.,1.));
#4017=DIRECTION('ref_axis',(1.,0.,0.));
#4018=DIRECTION('center_axis',(0.,0.,1.));
#4019=DIRECTION('ref_axis',(1.,0.,0.));
#4020=DIRECTION('center_axis',(0.,0.,1.));
#4021=DIRECTION('ref_axis',(1.,0.,0.));
#4022=DIRECTION('',(0.5,0.866025403784439,0.));
#4023=DIRECTION('',(1.,-3.29650746237182E-16,0.));
#4024=DIRECTION('',(0.5,-0.866025403784439,0.));
#4025=DIRECTION('',(-0.5,-0.866025403784439,0.));
#4026=DIRECTION('',(-1.,0.,0.));
#4027=DIRECTION('',(-0.5,0.866025403784439,0.));
#4028=DIRECTION('center_axis',(0.,0.,1.));
#4029=DIRECTION('ref_axis',(1.,0.,0.));
#4030=DIRECTION('center_axis',(-3.29650746237182E-16,-1.,0.));
#4031=DIRECTION('ref_axis',(1.,-3.29650746237182E-16,0.));
#4032=DIRECTION('',(0.,0.,1.));
#4033=DIRECTION('',(1.,-3.29650746237182E-16,0.));
#4034=DIRECTION('',(0.,0.,1.));
#4035=DIRECTION('center_axis',(-0.866025403784439,-0.5,0.));
#4036=DIRECTION('ref_axis',(0.5,-0.866025403784439,0.));
#4037=DIRECTION('',(0.5,-0.866025403784439,0.));
#4038=DIRECTION('',(0.,0.,1.));
#4039=DIRECTION('center_axis',(-0.866025403784439,0.5,0.));
#4040=DIRECTION('ref_axis',(-0.5,-0.866025403784439,0.));
#4041=DIRECTION('',(-0.5,-0.866025403784439,0.));
#4042=DIRECTION('',(0.,0.,1.));
#4043=DIRECTION('center_axis',(0.,1.,0.));
#4044=DIRECTION('ref_axis',(-1.,0.,0.));
#4045=DIRECTION('',(-1.,0.,0.));
#4046=DIRECTION('',(0.,0.,1.));
#4047=DIRECTION('center_axis',(0.866025403784439,0.5,0.));
#4048=DIRECTION('ref_axis',(-0.5,0.866025403784439,0.));
#4049=DIRECTION('',(-0.5,0.866025403784439,0.));
#4050=DIRECTION('',(0.,0.,1.));
#4051=DIRECTION('center_axis',(0.866025403784439,-0.5,0.));
#4052=DIRECTION('ref_axis',(0.5,0.866025403784439,0.));
#4053=DIRECTION('',(0.5,0.866025403784439,0.));
#4054=DIRECTION('center_axis',(0.,0.,1.));
#4055=DIRECTION('ref_axis',(1.,0.,0.));
#4056=DIRECTION('center_axis',(0.,0.,1.));
#4057=DIRECTION('ref_axis',(1.,0.,0.));
#4058=DIRECTION('',(0.,0.,-1.));
#4059=DIRECTION('center_axis',(0.,0.,-1.));
#4060=DIRECTION('ref_axis',(1.,0.,0.));
#4061=DIRECTION('center_axis',(0.,0.,1.));
#4062=DIRECTION('ref_axis',(1.,0.,0.));
#4063=DIRECTION('',(0.,0.,-1.));
#4064=DIRECTION('center_axis',(0.,0.,1.));
#4065=DIRECTION('ref_axis',(1.,0.,0.));
#4066=DIRECTION('center_axis',(0.,0.,1.));
#4067=DIRECTION('ref_axis',(1.,0.,0.));
#4068=DIRECTION('axis',(0.,0.,1.));
#4069=DIRECTION('refdir',(1.,0.,0.));
#4070=DIRECTION('center_axis',(0.,0.,1.));
#4071=DIRECTION('ref_axis',(1.,0.,0.));
#4072=DIRECTION('center_axis',(0.,0.,1.));
#4073=DIRECTION('ref_axis',(1.,0.,0.));
#4074=DIRECTION('',(0.,0.,1.));
#4075=DIRECTION('center_axis',(0.,0.,-1.));
#4076=DIRECTION('ref_axis',(1.,0.,0.));
#4077=DIRECTION('center_axis',(0.,0.,1.));
#4078=DIRECTION('ref_axis',(1.,0.,0.));
#4079=DIRECTION('center_axis',(0.,0.,1.));
#4080=DIRECTION('ref_axis',(1.,0.,0.));
#4081=DIRECTION('center_axis',(0.,0.,1.));
#4082=DIRECTION('ref_axis',(1.,0.,0.));
#4083=DIRECTION('',(0.5,0.866025403784439,0.));
#4084=DIRECTION('',(1.,-3.29650746237182E-16,0.));
#4085=DIRECTION('',(0.5,-0.866025403784439,0.));
#4086=DIRECTION('',(-0.5,-0.866025403784438,0.));
#4087=DIRECTION('',(-1.,0.,0.));
#4088=DIRECTION('',(-0.5,0.866025403784439,0.));
#4089=DIRECTION('center_axis',(0.,0.,1.));
#4090=DIRECTION('ref_axis',(1.,0.,0.));
#4091=DIRECTION('center_axis',(-3.29650746237182E-16,-1.,0.));
#4092=DIRECTION('ref_axis',(1.,-3.29650746237182E-16,0.));
#4093=DIRECTION('',(0.,0.,1.));
#4094=DIRECTION('',(1.,-3.29650746237182E-16,0.));
#4095=DIRECTION('',(0.,0.,1.));
#4096=DIRECTION('center_axis',(-0.866025403784439,-0.5,0.));
#4097=DIRECTION('ref_axis',(0.5,-0.866025403784439,0.));
#4098=DIRECTION('',(0.5,-0.866025403784439,0.));
#4099=DIRECTION('',(0.,0.,1.));
#4100=DIRECTION('center_axis',(-0.866025403784438,0.5,0.));
#4101=DIRECTION('ref_axis',(-0.5,-0.866025403784438,0.));
#4102=DIRECTION('',(-0.5,-0.866025403784438,0.));
#4103=DIRECTION('',(0.,0.,1.));
#4104=DIRECTION('center_axis',(0.,1.,0.));
#4105=DIRECTION('ref_axis',(-1.,0.,0.));
#4106=DIRECTION('',(-1.,0.,0.));
#4107=DIRECTION('',(0.,0.,1.));
#4108=DIRECTION('center_axis',(0.866025403784439,0.5,0.));
#4109=DIRECTION('ref_axis',(-0.5,0.866025403784439,0.));
#4110=DIRECTION('',(-0.5,0.866025403784439,0.));
#4111=DIRECTION('',(0.,0.,1.));
#4112=DIRECTION('center_axis',(0.866025403784439,-0.5,0.));
#4113=DIRECTION('ref_axis',(0.5,0.866025403784439,0.));
#4114=DIRECTION('',(0.5,0.866025403784439,0.));
#4115=DIRECTION('center_axis',(0.,0.,1.));
#4116=DIRECTION('ref_axis',(1.,0.,0.));
#4117=DIRECTION('center_axis',(0.,0.,1.));
#4118=DIRECTION('ref_axis',(1.,0.,0.));
#4119=DIRECTION('',(0.,0.,-1.));
#4120=DIRECTION('center_axis',(0.,0.,-1.));
#4121=DIRECTION('ref_axis',(1.,0.,0.));
#4122=DIRECTION('center_axis',(0.,0.,1.));
#4123=DIRECTION('ref_axis',(1.,0.,0.));
#4124=DIRECTION('',(0.,0.,-1.));
#4125=DIRECTION('center_axis',(0.,0.,1.));
#4126=DIRECTION('ref_axis',(1.,0.,0.));
#4127=DIRECTION('center_axis',(0.,0.,1.));
#4128=DIRECTION('ref_axis',(1.,0.,0.));
#4129=DIRECTION('axis',(0.,0.,1.));
#4130=DIRECTION('refdir',(1.,0.,0.));
#4131=DIRECTION('center_axis',(0.,0.,1.));
#4132=DIRECTION('ref_axis',(1.,0.,0.));
#4133=DIRECTION('center_axis',(0.,0.,1.));
#4134=DIRECTION('ref_axis',(1.,0.,0.));
#4135=DIRECTION('',(0.,0.,1.));
#4136=DIRECTION('center_axis',(0.,0.,-1.));
#4137=DIRECTION('ref_axis',(1.,0.,0.));
#4138=DIRECTION('center_axis',(0.,0.,1.));
#4139=DIRECTION('ref_axis',(1.,0.,0.));
#4140=DIRECTION('center_axis',(0.,0.,1.));
#4141=DIRECTION('ref_axis',(1.,0.,0.));
#4142=DIRECTION('',(0.,0.,1.));
#4143=DIRECTION('center_axis',(0.,0.,-1.));
#4144=DIRECTION('ref_axis',(1.,0.,0.));
#4145=DIRECTION('center_axis',(0.,0.,1.));
#4146=DIRECTION('ref_axis',(1.,0.,0.));
#4147=DIRECTION('center_axis',(0.,0.,1.));
#4148=DIRECTION('ref_axis',(1.,0.,0.));
#4149=DIRECTION('',(0.,0.,1.));
#4150=DIRECTION('center_axis',(0.,0.,-1.));
#4151=DIRECTION('ref_axis',(1.,0.,0.));
#4152=DIRECTION('center_axis',(0.,0.,1.));
#4153=DIRECTION('ref_axis',(1.,0.,0.));
#4154=DIRECTION('center_axis',(0.,0.,1.));
#4155=DIRECTION('ref_axis',(1.,0.,0.));
#4156=DIRECTION('',(0.,0.,1.));
#4157=DIRECTION('center_axis',(0.,0.,1.));
#4158=DIRECTION('ref_axis',(1.,0.,0.));
#4159=DIRECTION('center_axis',(0.,0.,1.));
#4160=DIRECTION('ref_axis',(1.,0.,0.));
#4161=DIRECTION('center_axis',(0.,0.,-1.));
#4162=DIRECTION('ref_axis',(1.,0.,0.));
#4163=DIRECTION('center_axis',(0.,0.,1.));
#4164=DIRECTION('ref_axis',(1.,0.,0.));
#4165=DIRECTION('center_axis',(0.,0.,1.));
#4166=DIRECTION('ref_axis',(1.,0.,0.));
#4167=DIRECTION('',(0.,0.,1.));
#4168=DIRECTION('center_axis',(0.,0.,1.));
#4169=DIRECTION('ref_axis',(1.,0.,0.));
#4170=DIRECTION('center_axis',(0.,0.,1.));
#4171=DIRECTION('ref_axis',(1.,0.,0.));
#4172=DIRECTION('center_axis',(0.,0.,-1.));
#4173=DIRECTION('ref_axis',(1.,0.,0.));
#4174=DIRECTION('center_axis',(0.,0.,1.));
#4175=DIRECTION('ref_axis',(1.,0.,0.));
#4176=DIRECTION('',(0.,0.,1.));
#4177=DIRECTION('center_axis',(0.,0.,-1.));
#4178=DIRECTION('ref_axis',(1.,0.,0.));
#4179=DIRECTION('center_axis',(0.,0.,1.));
#4180=DIRECTION('ref_axis',(1.,0.,0.));
#4181=DIRECTION('',(0.,0.,1.));
#4182=DIRECTION('center_axis',(0.,0.,-1.));
#4183=DIRECTION('ref_axis',(1.,0.,0.));
#4184=DIRECTION('center_axis',(0.,1.,0.));
#4185=DIRECTION('ref_axis',(-1.,0.,0.));
#4186=DIRECTION('',(-1.,0.,0.));
#4187=DIRECTION('',(0.,0.,1.));
#4188=DIRECTION('',(-1.,0.,0.));
#4189=DIRECTION('',(0.,0.,1.));
#4190=DIRECTION('center_axis',(1.,0.,0.));
#4191=DIRECTION('ref_axis',(0.,1.,0.));
#4192=DIRECTION('',(0.,1.,0.));
#4193=DIRECTION('',(0.,1.,0.));
#4194=DIRECTION('',(0.,0.,1.));
#4195=DIRECTION('center_axis',(0.,-1.,0.));
#4196=DIRECTION('ref_axis',(1.,0.,0.));
#4197=DIRECTION('',(1.,0.,0.));
#4198=DIRECTION('',(1.,0.,0.));
#4199=DIRECTION('',(0.,0.,1.));
#4200=DIRECTION('center_axis',(-1.,0.,0.));
#4201=DIRECTION('ref_axis',(0.,-1.,0.));
#4202=DIRECTION('',(0.,-1.,0.));
#4203=DIRECTION('',(0.,-1.,0.));
#4204=DIRECTION('center_axis',(0.,0.,1.));
#4205=DIRECTION('ref_axis',(1.,0.,0.));
#4206=DIRECTION('center_axis',(0.,0.,1.));
#4207=DIRECTION('ref_axis',(1.,0.,0.));
#4208=DIRECTION('axis',(0.,0.,1.));
#4209=DIRECTION('refdir',(1.,0.,0.));
#4210=DIRECTION('center_axis',(0.,0.,1.));
#4211=DIRECTION('ref_axis',(1.,0.,0.));
#4212=DIRECTION('center_axis',(0.,0.,1.));
#4213=DIRECTION('ref_axis',(1.,0.,0.));
#4214=DIRECTION('',(0.,0.,1.));
#4215=DIRECTION('center_axis',(0.,0.,-1.));
#4216=DIRECTION('ref_axis',(1.,0.,0.));
#4217=DIRECTION('center_axis',(0.,0.,1.));
#4218=DIRECTION('ref_axis',(1.,0.,0.));
#4219=DIRECTION('center_axis',(0.,0.,1.));
#4220=DIRECTION('ref_axis',(1.,0.,0.));
#4221=DIRECTION('',(0.,0.,1.));
#4222=DIRECTION('center_axis',(0.,0.,-1.));
#4223=DIRECTION('ref_axis',(1.,0.,0.));
#4224=DIRECTION('center_axis',(0.,0.,1.));
#4225=DIRECTION('ref_axis',(1.,0.,0.));
#4226=DIRECTION('center_axis',(0.,0.,1.));
#4227=DIRECTION('ref_axis',(1.,0.,0.));
#4228=DIRECTION('',(0.,0.,1.));
#4229=DIRECTION('center_axis',(0.,0.,-1.));
#4230=DIRECTION('ref_axis',(1.,0.,0.));
#4231=DIRECTION('center_axis',(0.,0.,1.));
#4232=DIRECTION('ref_axis',(1.,0.,0.));
#4233=DIRECTION('center_axis',(0.,0.,1.));
#4234=DIRECTION('ref_axis',(1.,0.,0.));
#4235=DIRECTION('',(0.,0.,1.));
#4236=DIRECTION('center_axis',(0.,0.,1.));
#4237=DIRECTION('ref_axis',(1.,0.,0.));
#4238=DIRECTION('center_axis',(0.,0.,1.));
#4239=DIRECTION('ref_axis',(1.,0.,0.));
#4240=DIRECTION('center_axis',(0.,0.,-1.));
#4241=DIRECTION('ref_axis',(1.,0.,0.));
#4242=DIRECTION('center_axis',(0.,0.,1.));
#4243=DIRECTION('ref_axis',(1.,0.,0.));
#4244=DIRECTION('center_axis',(0.,0.,1.));
#4245=DIRECTION('ref_axis',(1.,0.,0.));
#4246=DIRECTION('',(0.,0.,1.));
#4247=DIRECTION('center_axis',(0.,0.,1.));
#4248=DIRECTION('ref_axis',(1.,0.,0.));
#4249=DIRECTION('center_axis',(0.,0.,1.));
#4250=DIRECTION('ref_axis',(1.,0.,0.));
#4251=DIRECTION('center_axis',(0.,0.,-1.));
#4252=DIRECTION('ref_axis',(1.,0.,0.));
#4253=DIRECTION('center_axis',(0.,0.,1.));
#4254=DIRECTION('ref_axis',(1.,0.,0.));
#4255=DIRECTION('',(0.,0.,1.));
#4256=DIRECTION('center_axis',(0.,0.,-1.));
#4257=DIRECTION('ref_axis',(1.,0.,0.));
#4258=DIRECTION('center_axis',(0.,0.,1.));
#4259=DIRECTION('ref_axis',(1.,0.,0.));
#4260=DIRECTION('',(0.,0.,1.));
#4261=DIRECTION('center_axis',(0.,0.,-1.));
#4262=DIRECTION('ref_axis',(1.,0.,0.));
#4263=DIRECTION('center_axis',(0.,1.,0.));
#4264=DIRECTION('ref_axis',(-1.,0.,0.));
#4265=DIRECTION('',(-1.,0.,0.));
#4266=DIRECTION('',(0.,0.,1.));
#4267=DIRECTION('',(-1.,0.,0.));
#4268=DIRECTION('',(0.,0.,1.));
#4269=DIRECTION('center_axis',(1.,0.,0.));
#4270=DIRECTION('ref_axis',(0.,1.,0.));
#4271=DIRECTION('',(0.,1.,0.));
#4272=DIRECTION('',(0.,1.,0.));
#4273=DIRECTION('',(0.,0.,1.));
#4274=DIRECTION('center_axis',(0.,-1.,0.));
#4275=DIRECTION('ref_axis',(1.,0.,0.));
#4276=DIRECTION('',(1.,0.,0.));
#4277=DIRECTION('',(1.,0.,0.));
#4278=DIRECTION('',(0.,0.,1.));
#4279=DIRECTION('center_axis',(-1.,0.,0.));
#4280=DIRECTION('ref_axis',(0.,-1.,0.));
#4281=DIRECTION('',(0.,-1.,0.));
#4282=DIRECTION('',(0.,-1.,0.));
#4283=DIRECTION('center_axis',(0.,0.,1.));
#4284=DIRECTION('ref_axis',(1.,0.,0.));
#4285=DIRECTION('center_axis',(0.,0.,1.));
#4286=DIRECTION('ref_axis',(1.,0.,0.));
#4287=DIRECTION('axis',(0.,0.,1.));
#4288=DIRECTION('refdir',(1.,0.,0.));
#4289=DIRECTION('center_axis',(1.14015052621434E-31,1.,-1.55447022770527E-24));
#4290=DIRECTION('ref_axis',(-1.,1.10933564796705E-31,5.55111512312579E-17));
#4291=DIRECTION('center_axis',(-1.14015052621434E-31,-1.,1.55447022770527E-24));
#4292=DIRECTION('ref_axis',(1.,0.,0.));
#4293=DIRECTION('center_axis',(1.14015052621434E-31,1.,-1.55447022770527E-24));
#4294=DIRECTION('ref_axis',(1.,0.,0.));
#4295=DIRECTION('center_axis',(0.,-1.,0.));
#4296=DIRECTION('ref_axis',(1.,0.,0.));
#4297=DIRECTION('center_axis',(0.,-1.,0.));
#4298=DIRECTION('ref_axis',(1.,0.,0.));
#4299=DIRECTION('',(0.,1.,0.));
#4300=DIRECTION('center_axis',(0.,1.,0.));
#4301=DIRECTION('ref_axis',(1.,0.,0.));
#4302=DIRECTION('',(-0.5,0.,0.866025403784439));
#4303=DIRECTION('',(-1.,0.,-3.29650746237182E-16));
#4304=DIRECTION('',(-0.5,0.,-0.866025403784439));
#4305=DIRECTION('',(0.5,0.,-0.866025403784438));
#4306=DIRECTION('',(1.,0.,0.));
#4307=DIRECTION('',(0.5,0.,0.866025403784439));
#4308=DIRECTION('center_axis',(0.,-1.,0.));
#4309=DIRECTION('ref_axis',(1.,0.,0.));
#4310=DIRECTION('center_axis',(0.,1.,0.));
#4311=DIRECTION('ref_axis',(1.,0.,0.));
#4312=DIRECTION('',(0.5,0.,-0.866025403784439));
#4313=DIRECTION('',(-0.5,0.,-0.866025403784439));
#4314=DIRECTION('',(-1.,0.,0.));
#4315=DIRECTION('',(-0.5,0.,0.866025403784438));
#4316=DIRECTION('',(0.5,0.,0.866025403784439));
#4317=DIRECTION('',(1.,0.,3.29650746237182E-16));
#4318=DIRECTION('center_axis',(0.,1.,0.));
#4319=DIRECTION('ref_axis',(1.,0.,0.));
#4320=DIRECTION('center_axis',(-3.29650746237182E-16,0.,1.));
#4321=DIRECTION('ref_axis',(1.,0.,3.29650746237182E-16));
#4322=DIRECTION('',(0.,-1.,0.));
#4323=DIRECTION('',(0.,1.,0.));
#4324=DIRECTION('center_axis',(-0.866025403784439,0.,0.5));
#4325=DIRECTION('ref_axis',(0.5,0.,0.866025403784439));
#4326=DIRECTION('',(0.,1.,0.));
#4327=DIRECTION('center_axis',(-0.866025403784439,0.,-0.5));
#4328=DIRECTION('ref_axis',(-0.5,0.,0.866025403784439));
#4329=DIRECTION('',(0.,1.,0.));
#4330=DIRECTION('center_axis',(0.,0.,-1.));
#4331=DIRECTION('ref_axis',(-1.,0.,0.));
#4332=DIRECTION('',(0.,1.,0.));
#4333=DIRECTION('center_axis',(0.866025403784439,0.,-0.5));
#4334=DIRECTION('ref_axis',(-0.5,0.,-0.866025403784439));
#4335=DIRECTION('',(0.,1.,0.));
#4336=DIRECTION('center_axis',(0.866025403784439,0.,0.5));
#4337=DIRECTION('ref_axis',(0.5,0.,-0.866025403784439));
#4338=DIRECTION('center_axis',(0.,-1.,0.));
#4339=DIRECTION('ref_axis',(1.,0.,0.));
#4340=DIRECTION('',(0.,1.,0.));
#4341=DIRECTION('center_axis',(0.,-1.,0.));
#4342=DIRECTION('ref_axis',(1.,0.,0.));
#4343=DIRECTION('center_axis',(0.,-1.,0.));
#4344=DIRECTION('ref_axis',(1.,0.,0.));
#4345=DIRECTION('',(0.,1.,0.));
#4346=DIRECTION('center_axis',(0.,1.,0.));
#4347=DIRECTION('ref_axis',(1.,0.,0.));
#4348=DIRECTION('center_axis',(0.,-1.,0.));
#4349=DIRECTION('ref_axis',(1.,0.,0.));
#4350=DIRECTION('',(-0.707106781186547,0.707106781186548,-8.65956056235493E-17));
#4351=DIRECTION('center_axis',(0.,-1.,0.));
#4352=DIRECTION('ref_axis',(0.,0.,-1.));
#4353=DIRECTION('axis',(0.,0.,1.));
#4354=DIRECTION('refdir',(1.,0.,0.));
#4355=DIRECTION('center_axis',(1.,0.,0.));
#4356=DIRECTION('ref_axis',(0.,0.,-1.));
#4357=DIRECTION('center_axis',(1.,0.,0.));
#4358=DIRECTION('ref_axis',(0.,0.,-1.));
#4359=DIRECTION('',(1.,0.,0.));
#4360=DIRECTION('center_axis',(1.,0.,0.));
#4361=DIRECTION('ref_axis',(0.,0.,-1.));
#4362=DIRECTION('center_axis',(1.,0.,0.));
#4363=DIRECTION('ref_axis',(0.,0.,-1.));
#4364=DIRECTION('center_axis',(1.,0.,0.));
#4365=DIRECTION('ref_axis',(0.,0.,-1.));
#4366=DIRECTION('',(0.,0.5,0.866025403784439));
#4367=DIRECTION('',(0.,1.,-4.39534328316243E-16));
#4368=DIRECTION('',(0.,0.5,-0.866025403784439));
#4369=DIRECTION('',(0.,-0.5,-0.866025403784439));
#4370=DIRECTION('',(0.,-1.,0.));
#4371=DIRECTION('',(0.,-0.5,0.866025403784439));
#4372=DIRECTION('center_axis',(0.,-4.39534328316243E-16,-1.));
#4373=DIRECTION('ref_axis',(0.,1.,-4.39534328316243E-16));
#4374=DIRECTION('',(1.,0.,0.));
#4375=DIRECTION('',(0.,1.,-4.39534328316243E-16));
#4376=DIRECTION('',(1.,0.,0.));
#4377=DIRECTION('center_axis',(0.,-0.866025403784439,-0.5));
#4378=DIRECTION('ref_axis',(0.,0.5,-0.866025403784439));
#4379=DIRECTION('',(0.,0.5,-0.866025403784439));
#4380=DIRECTION('',(1.,0.,0.));
#4381=DIRECTION('center_axis',(0.,-0.866025403784439,0.5));
#4382=DIRECTION('ref_axis',(0.,-0.5,-0.866025403784439));
#4383=DIRECTION('',(0.,-0.5,-0.866025403784439));
#4384=DIRECTION('',(1.,0.,0.));
#4385=DIRECTION('center_axis',(0.,0.,1.));
#4386=DIRECTION('ref_axis',(0.,-1.,0.));
#4387=DIRECTION('',(0.,-1.,0.));
#4388=DIRECTION('',(1.,0.,0.));
#4389=DIRECTION('center_axis',(0.,0.866025403784439,0.5));
#4390=DIRECTION('ref_axis',(0.,-0.5,0.866025403784439));
#4391=DIRECTION('',(0.,-0.5,0.866025403784439));
#4392=DIRECTION('',(1.,0.,0.));
#4393=DIRECTION('center_axis',(0.,0.866025403784439,-0.5));
#4394=DIRECTION('ref_axis',(0.,0.5,0.866025403784439));
#4395=DIRECTION('',(0.,0.5,0.866025403784439));
#4396=DIRECTION('center_axis',(1.,0.,0.));
#4397=DIRECTION('ref_axis',(0.,0.,-1.));
#4398=DIRECTION('axis',(0.,0.,1.));
#4399=DIRECTION('refdir',(1.,0.,0.));
#4400=DIRECTION('axis',(0.,0.,1.));
#4401=DIRECTION('refdir',(1.,0.,0.));
#4402=DIRECTION('center_axis',(0.,1.,0.));
#4403=DIRECTION('ref_axis',(1.,0.,0.));
#4404=DIRECTION('center_axis',(0.,1.,0.));
#4405=DIRECTION('ref_axis',(1.,0.,0.));
#4406=DIRECTION('',(0.,1.,0.));
#4407=DIRECTION('center_axis',(0.,-1.,0.));
#4408=DIRECTION('ref_axis',(1.,0.,0.));
#4409=DIRECTION('center_axis',(0.,1.,0.));
#4410=DIRECTION('ref_axis',(1.,0.,0.));
#4411=DIRECTION('center_axis',(0.,1.,0.));
#4412=DIRECTION('ref_axis',(1.,0.,0.));
#4413=DIRECTION('center_axis',(0.,1.,0.));
#4414=DIRECTION('ref_axis',(1.,0.,0.));
#4415=DIRECTION('',(0.5,0.,-0.866025403784439));
#4416=DIRECTION('',(-0.5,0.,-0.866025403784439));
#4417=DIRECTION('',(-1.,0.,-1.60246890531964E-16));
#4418=DIRECTION('',(-0.5,0.,0.866025403784439));
#4419=DIRECTION('',(0.5,0.,0.866025403784439));
#4420=DIRECTION('',(1.,0.,1.60246890531964E-16));
#4421=DIRECTION('center_axis',(0.,-1.,0.));
#4422=DIRECTION('ref_axis',(1.,0.,0.));
#4423=DIRECTION('center_axis',(0.,1.,0.));
#4424=DIRECTION('ref_axis',(1.,0.,0.));
#4425=DIRECTION('',(0.5,0.,-0.866025403784439));
#4426=DIRECTION('',(1.,0.,1.60246890531964E-16));
#4427=DIRECTION('',(0.5,0.,0.866025403784439));
#4428=DIRECTION('',(-0.5,0.,0.866025403784439));
#4429=DIRECTION('',(-1.,0.,-1.60246890531964E-16));
#4430=DIRECTION('',(-0.5,0.,-0.866025403784439));
#4431=DIRECTION('center_axis',(0.,-1.,0.));
#4432=DIRECTION('ref_axis',(1.,0.,0.));
#4433=DIRECTION('center_axis',(-1.60246890531964E-16,0.,1.));
#4434=DIRECTION('ref_axis',(1.,0.,1.60246890531964E-16));
#4435=DIRECTION('',(0.,1.,0.));
#4436=DIRECTION('',(0.,1.,0.));
#4437=DIRECTION('center_axis',(-0.866025403784439,0.,0.5));
#4438=DIRECTION('ref_axis',(0.5,0.,0.866025403784439));
#4439=DIRECTION('',(0.,1.,0.));
#4440=DIRECTION('center_axis',(-0.866025403784439,0.,-0.5));
#4441=DIRECTION('ref_axis',(-0.5,0.,0.866025403784439));
#4442=DIRECTION('',(0.,1.,0.));
#4443=DIRECTION('center_axis',(1.60246890531964E-16,0.,-1.));
#4444=DIRECTION('ref_axis',(-1.,0.,-1.60246890531964E-16));
#4445=DIRECTION('',(0.,1.,0.));
#4446=DIRECTION('center_axis',(0.866025403784439,0.,-0.5));
#4447=DIRECTION('ref_axis',(-0.5,0.,-0.866025403784439));
#4448=DIRECTION('',(0.,1.,0.));
#4449=DIRECTION('center_axis',(0.866025403784439,0.,0.5));
#4450=DIRECTION('ref_axis',(0.5,0.,-0.866025403784439));
#4451=DIRECTION('center_axis',(0.,1.,0.));
#4452=DIRECTION('ref_axis',(0.,0.,1.));
#4453=DIRECTION('center_axis',(0.,-1.,0.));
#4454=DIRECTION('ref_axis',(1.,0.,0.));
#4455=DIRECTION('center_axis',(0.,-1.,0.));
#4456=DIRECTION('ref_axis',(1.,0.,0.));
#4457=DIRECTION('',(0.,1.,0.));
#4458=DIRECTION('center_axis',(0.,-1.,0.));
#4459=DIRECTION('ref_axis',(1.,0.,0.));
#4460=DIRECTION('center_axis',(0.,1.,0.));
#4461=DIRECTION('ref_axis',(0.,0.,1.));
#4462=DIRECTION('center_axis',(0.,-1.,0.));
#4463=DIRECTION('ref_axis',(1.,0.,0.));
#4464=DIRECTION('center_axis',(0.,-1.,0.));
#4465=DIRECTION('ref_axis',(1.,0.,0.));
#4466=DIRECTION('',(0.,1.,0.));
#4467=DIRECTION('center_axis',(0.,-1.,0.));
#4468=DIRECTION('ref_axis',(1.,0.,0.));
#4469=DIRECTION('center_axis',(0.,-1.,0.));
#4470=DIRECTION('ref_axis',(1.,0.,0.));
#4471=DIRECTION('',(0.,1.,0.));
#4472=DIRECTION('center_axis',(0.,-1.,0.));
#4473=DIRECTION('ref_axis',(0.,0.,-1.));
#4474=DIRECTION('center_axis',(0.,-1.,0.));
#4475=DIRECTION('ref_axis',(1.,0.,0.));
#4476=DIRECTION('center_axis',(0.,-1.,0.));
#4477=DIRECTION('ref_axis',(1.,0.,0.));
#4478=DIRECTION('',(0.,1.,0.));
#4479=DIRECTION('axis',(0.,0.,1.));
#4480=DIRECTION('refdir',(1.,0.,0.));
#4481=DIRECTION('center_axis',(0.,1.,0.));
#4482=DIRECTION('ref_axis',(0.,0.,1.));
#4483=DIRECTION('center_axis',(0.,-1.,0.));
#4484=DIRECTION('ref_axis',(1.,0.,0.));
#4485=DIRECTION('center_axis',(0.,-1.,0.));
#4486=DIRECTION('ref_axis',(1.,0.,0.));
#4487=DIRECTION('center_axis',(0.,-1.,0.));
#4488=DIRECTION('ref_axis',(1.,0.,0.));
#4489=DIRECTION('center_axis',(0.,-1.,0.));
#4490=DIRECTION('ref_axis',(1.,0.,0.));
#4491=DIRECTION('',(0.,1.,0.));
#4492=DIRECTION('center_axis',(0.,-1.,0.));
#4493=DIRECTION('ref_axis',(0.,0.,-1.));
#4494=DIRECTION('center_axis',(0.,-1.,0.));
#4495=DIRECTION('ref_axis',(1.,0.,0.));
#4496=DIRECTION('center_axis',(0.,-1.,0.));
#4497=DIRECTION('ref_axis',(1.,0.,0.));
#4498=DIRECTION('center_axis',(0.,-1.,0.));
#4499=DIRECTION('ref_axis',(1.,0.,0.));
#4500=DIRECTION('',(0.,1.,0.));
#4501=DIRECTION('center_axis',(0.,-1.,0.));
#4502=DIRECTION('ref_axis',(0.,0.,-1.));
#4503=DIRECTION('center_axis',(0.,-1.,0.));
#4504=DIRECTION('ref_axis',(1.,0.,0.));
#4505=DIRECTION('center_axis',(0.,-1.,0.));
#4506=DIRECTION('ref_axis',(1.,0.,0.));
#4507=DIRECTION('',(0.,1.,0.));
#4508=DIRECTION('',(0.,0.,1.));
#4509=DIRECTION('',(1.,0.,0.));
#4510=DIRECTION('',(0.,0.,1.));
#4511=DIRECTION('',(1.,0.,0.));
#4512=DIRECTION('axis',(0.,0.,1.));
#4513=DIRECTION('refdir',(1.,0.,0.));
#4514=DIRECTION('center_axis',(6.12323399573679E-17,0.,1.));
#4515=DIRECTION('ref_axis',(1.,0.,0.));
#4516=DIRECTION('center_axis',(0.,-1.,0.));
#4517=DIRECTION('ref_axis',(1.,0.,0.));
#4518=DIRECTION('center_axis',(0.,-1.,0.));
#4519=DIRECTION('ref_axis',(1.,0.,0.));
#4520=DIRECTION('center_axis',(0.,-1.,0.));
#4521=DIRECTION('ref_axis',(1.,0.,0.));
#4522=DIRECTION('',(0.,1.,0.));
#4523=DIRECTION('center_axis',(0.,1.,0.));
#4524=DIRECTION('ref_axis',(1.,0.,0.));
#4525=DIRECTION('center_axis',(0.,-1.,0.));
#4526=DIRECTION('ref_axis',(1.,0.,0.));
#4527=DIRECTION('',(-0.707106781186548,0.707106781186547,-8.65956056235493E-17));
#4528=DIRECTION('center_axis',(0.,-1.,0.));
#4529=DIRECTION('ref_axis',(0.,0.,-1.));
#4530=DIRECTION('axis',(0.,0.,1.));
#4531=DIRECTION('refdir',(1.,0.,0.));
#4532=DIRECTION('center_axis',(0.,1.,0.));
#4533=DIRECTION('ref_axis',(1.,0.,0.));
#4534=DIRECTION('center_axis',(0.,-1.,0.));
#4535=DIRECTION('ref_axis',(1.,0.,0.));
#4536=DIRECTION('',(0.,-1.,0.));
#4537=DIRECTION('center_axis',(0.,-1.,0.));
#4538=DIRECTION('ref_axis',(1.,0.,0.));
#4539=DIRECTION('center_axis',(0.,1.,0.));
#4540=DIRECTION('ref_axis',(1.,0.,0.));
#4541=DIRECTION('center_axis',(0.,1.,0.));
#4542=DIRECTION('ref_axis',(1.,0.,0.));
#4543=DIRECTION('',(0.,-1.,0.));
#4544=DIRECTION('center_axis',(0.,1.,0.));
#4545=DIRECTION('ref_axis',(1.,0.,0.));
#4546=DIRECTION('center_axis',(0.,1.,0.));
#4547=DIRECTION('ref_axis',(1.,0.,0.));
#4548=DIRECTION('center_axis',(0.,1.,0.));
#4549=DIRECTION('ref_axis',(1.,0.,0.));
#4550=DIRECTION('axis',(0.,0.,1.));
#4551=DIRECTION('refdir',(1.,0.,0.));
#4552=DIRECTION('center_axis',(0.,-1.,0.));
#4553=DIRECTION('ref_axis',(1.,0.,0.));
#4554=DIRECTION('center_axis',(0.,1.,0.));
#4555=DIRECTION('ref_axis',(1.,0.,0.));
#4556=DIRECTION('',(0.,1.,0.));
#4557=DIRECTION('center_axis',(0.,-1.,0.));
#4558=DIRECTION('ref_axis',(1.,0.,0.));
#4559=DIRECTION('center_axis',(0.,1.,0.));
#4560=DIRECTION('ref_axis',(1.,0.,0.));
#4561=DIRECTION('center_axis',(0.,-1.,0.));
#4562=DIRECTION('ref_axis',(1.,0.,0.));
#4563=DIRECTION('',(-0.707106781186547,0.707106781186548,-8.65956056235493E-17));
#4564=DIRECTION('center_axis',(0.,-1.,0.));
#4565=DIRECTION('ref_axis',(0.,0.,-1.));
#4566=DIRECTION('center_axis',(0.,-1.,0.));
#4567=DIRECTION('ref_axis',(1.,0.,0.));
#4568=DIRECTION('center_axis',(0.,1.,0.));
#4569=DIRECTION('ref_axis',(1.,0.,0.));
#4570=DIRECTION('',(-0.866025403784439,-0.5,-1.06057523872491E-16));
#4571=DIRECTION('center_axis',(1.92296268638356E-16,0.,-1.));
#4572=DIRECTION('ref_axis',(-1.,0.,-1.92296268638356E-16));
#4573=DIRECTION('',(0.,1.,0.));
#4574=DIRECTION('',(-1.,0.,-1.92296268638356E-16));
#4575=DIRECTION('',(0.,1.,0.));
#4576=DIRECTION('center_axis',(0.866025403784439,0.,-0.5));
#4577=DIRECTION('ref_axis',(-0.5,0.,-0.866025403784439));
#4578=DIRECTION('',(0.,1.,0.));
#4579=DIRECTION('',(-0.5,0.,-0.866025403784439));
#4580=DIRECTION('center_axis',(0.866025403784439,0.,0.5));
#4581=DIRECTION('ref_axis',(0.5,0.,-0.866025403784439));
#4582=DIRECTION('',(0.,1.,0.));
#4583=DIRECTION('',(0.5,0.,-0.866025403784439));
#4584=DIRECTION('center_axis',(-1.92296268638356E-16,0.,1.));
#4585=DIRECTION('ref_axis',(1.,0.,1.92296268638356E-16));
#4586=DIRECTION('',(0.,1.,0.));
#4587=DIRECTION('',(1.,0.,1.92296268638356E-16));
#4588=DIRECTION('center_axis',(-0.866025403784439,0.,0.5));
#4589=DIRECTION('ref_axis',(0.5,0.,0.866025403784439));
#4590=DIRECTION('',(0.,1.,0.));
#4591=DIRECTION('',(0.5,0.,0.866025403784439));
#4592=DIRECTION('center_axis',(-0.866025403784439,0.,-0.5));
#4593=DIRECTION('ref_axis',(-0.5,0.,0.866025403784439));
#4594=DIRECTION('',(-0.5,0.,0.866025403784438));
#4595=DIRECTION('center_axis',(0.,1.,0.));
#4596=DIRECTION('ref_axis',(0.,0.,1.));
#4597=DIRECTION('center_axis',(0.,1.,0.));
#4598=DIRECTION('ref_axis',(1.,0.,0.));
#4599=DIRECTION('',(0.,0.,1.));
#4600=DIRECTION('',(1.,0.,0.));
#4601=DIRECTION('',(0.,0.,1.));
#4602=DIRECTION('',(1.,0.,0.));
#4603=DIRECTION('',(0.,0.,1.));
#4604=DIRECTION('',(1.,0.,0.));
#4605=DIRECTION('',(0.,0.,1.));
#4606=DIRECTION('',(1.,0.,0.));
#4607=DIRECTION('',(0.,0.,1.));
#4608=DIRECTION('',(1.,0.,0.));
#4609=DIRECTION('',(0.,0.,1.));
#4610=DIRECTION('',(1.,0.,0.));
#4611=DIRECTION('',(0.,0.,1.));
#4612=DIRECTION('',(1.,0.,0.));
#4613=DIRECTION('',(1.10657474353458E-16,-1.62048040804624E-16,1.));
#4614=DIRECTION('',(2.22044604925031E-16,-1.,5.55111512312578E-17));
#4615=DIRECTION('',(0.,0.,1.));
#4616=DIRECTION('',(1.,0.,0.));
#4617=DIRECTION('',(0.,-1.,2.22044604925031E-16));
#4618=DIRECTION('',(1.,0.,0.));
#4619=DIRECTION('',(0.,-1.,2.22044604925031E-16));
#4620=DIRECTION('',(1.,0.,0.));
#4621=DIRECTION('',(0.,-1.,2.22044604925031E-16));
#4622=DIRECTION('',(1.,0.,0.));
#4623=DIRECTION('',(0.,-1.,2.22044604925031E-16));
#4624=DIRECTION('',(1.,0.,0.));
#4625=DIRECTION('',(0.,-1.,2.22044604925031E-16));
#4626=DIRECTION('',(1.,0.,0.));
#4627=DIRECTION('',(0.,1.,2.22044604925031E-16));
#4628=DIRECTION('',(1.,0.,0.));
#4629=DIRECTION('',(0.,1.,2.22044604925031E-16));
#4630=DIRECTION('',(1.,0.,0.));
#4631=DIRECTION('',(0.,1.,2.22044604925031E-16));
#4632=DIRECTION('',(1.,0.,0.));
#4633=DIRECTION('',(0.,1.,2.22044604925031E-16));
#4634=DIRECTION('',(1.,0.,0.));
#4635=DIRECTION('',(0.,-1.,2.22044604925031E-16));
#4636=DIRECTION('',(1.,0.,0.));
#4637=DIRECTION('',(0.,1.,2.22044604925031E-16));
#4638=DIRECTION('',(1.,0.,0.));
#4639=DIRECTION('',(0.,1.,2.22044604925031E-16));
#4640=DIRECTION('',(1.,0.,0.));
#4641=DIRECTION('',(0.,1.,2.22044604925031E-16));
#4642=DIRECTION('',(1.,0.,0.));
#4643=DIRECTION('',(0.,1.,2.22044604925031E-16));
#4644=DIRECTION('',(1.,0.,0.));
#4645=CARTESIAN_POINT('',(0.,0.,0.));
#4646=CARTESIAN_POINT('',(0.,0.,0.));
#4647=CARTESIAN_POINT('Origin',(3.75,0.,3.8));
#4648=CARTESIAN_POINT('',(4.05,-0.615812471455394,3.8));
#4649=CARTESIAN_POINT('',(3.45,-0.615812471455394,3.8));
#4650=CARTESIAN_POINT('',(-5.5,-0.615812471455394,3.8));
#4651=CARTESIAN_POINT('Origin',(3.75,0.,3.8));
#4652=CARTESIAN_POINT('Origin',(3.75,0.,3.8));
#4653=CARTESIAN_POINT('',(4.05,0.615812471455394,3.8));
#4654=CARTESIAN_POINT('',(4.435,-8.38883057415936E-17,4.185));
#4655=CARTESIAN_POINT('Origin',(3.75,0.,3.5));
#4656=CARTESIAN_POINT('Origin',(3.75,0.,3.5));
#4657=CARTESIAN_POINT('',(3.065,-8.38883057415936E-17,4.185));
#4658=CARTESIAN_POINT('Origin',(3.75,0.,3.5));
#4659=CARTESIAN_POINT('',(3.065,8.38883057415936E-17,5.));
#4660=CARTESIAN_POINT('',(3.065,-8.38883057415936E-17,3.8));
#4661=CARTESIAN_POINT('Origin',(3.75,0.,5.));
#4662=CARTESIAN_POINT('',(3.45,0.615812471455394,3.8));
#4663=CARTESIAN_POINT('Origin',(3.75,0.,3.5));
#4664=CARTESIAN_POINT('Origin',(3.75,0.,3.8));
#4665=CARTESIAN_POINT('Origin',(1.25,0.,3.8));
#4666=CARTESIAN_POINT('',(0.95,0.615812471455394,3.8));
#4667=CARTESIAN_POINT('',(1.55,0.615812471455394,3.8));
#4668=CARTESIAN_POINT('',(-5.5,0.615812471455394,3.8));
#4669=CARTESIAN_POINT('Origin',(1.25,0.,3.8));
#4670=CARTESIAN_POINT('Origin',(-1.25,0.,3.8));
#4671=CARTESIAN_POINT('',(-1.55,0.615812471455394,3.8));
#4672=CARTESIAN_POINT('',(-0.95,0.615812471455394,3.8));
#4673=CARTESIAN_POINT('',(-5.5,0.615812471455394,3.8));
#4674=CARTESIAN_POINT('Origin',(-1.25,0.,3.8));
#4675=CARTESIAN_POINT('Origin',(-3.75,0.,3.8));
#4676=CARTESIAN_POINT('',(-4.05,-0.615812471455394,3.8));
#4677=CARTESIAN_POINT('',(-4.435,-8.38883057415937E-17,4.185));
#4678=CARTESIAN_POINT('Origin',(-3.75,0.,3.5));
#4679=CARTESIAN_POINT('',(-4.435,8.38883057415937E-17,5.));
#4680=CARTESIAN_POINT('',(-4.435,-8.38883057415937E-17,3.8));
#4681=CARTESIAN_POINT('Origin',(-3.75,0.,5.));
#4682=CARTESIAN_POINT('',(-4.05,0.615812471455394,3.8));
#4683=CARTESIAN_POINT('Origin',(-3.75,0.,3.5));
#4684=CARTESIAN_POINT('',(-3.45,0.615812471455394,3.8));
#4685=CARTESIAN_POINT('Origin',(-3.75,0.,3.8));
#4686=CARTESIAN_POINT('',(-3.065,-8.38883057415936E-17,4.185));
#4687=CARTESIAN_POINT('Origin',(-3.75,0.,3.5));
#4688=CARTESIAN_POINT('',(-3.45,-0.615812471455394,3.8));
#4689=CARTESIAN_POINT('Origin',(-3.75,0.,3.5));
#4690=CARTESIAN_POINT('Origin',(-3.75,0.,3.8));
#4691=CARTESIAN_POINT('Origin',(4.5,0.,0.9));
#4692=CARTESIAN_POINT('',(4.295,-2.51052593825207E-17,2.));
#4693=CARTESIAN_POINT('Origin',(4.5,0.,2.));
#4694=CARTESIAN_POINT('',(4.295,-5.61373578735315E-18,2.815));
#4695=CARTESIAN_POINT('',(4.295,-2.51052593825207E-17,0.9));
#4696=CARTESIAN_POINT('',(4.5,-0.205,2.84639461446527));
#4697=CARTESIAN_POINT('Ctrl Pts',(4.5,-0.205,2.84639461446527));
#4698=CARTESIAN_POINT('Ctrl Pts',(4.4740836410313,-0.205,2.84639461446527));
#4699=CARTESIAN_POINT('Ctrl Pts',(4.4465572469413,-0.199787945222222,2.84469184063064));
#4700=CARTESIAN_POINT('Ctrl Pts',(4.3961018032059,-0.178819800999948,2.83866235487196));
#4701=CARTESIAN_POINT('Ctrl Pts',(4.37315766716202,-0.163071447448502,2.83443540996919));
#4702=CARTESIAN_POINT('Ctrl Pts',(4.33693389431385,-0.12684767460033,2.82659225921127));
#4703=CARTESIAN_POINT('Ctrl Pts',(4.32118140385364,-0.103901367097065,2.82244952053683));
#4704=CARTESIAN_POINT('Ctrl Pts',(4.3002102058406,-0.0534380328956992,2.81661539166144));
#4705=CARTESIAN_POINT('Ctrl Pts',(4.295,-0.0259087165500479,2.815));
#4706=CARTESIAN_POINT('Ctrl Pts',(4.295,-6.24500451351651E-17,2.815));
#4707=CARTESIAN_POINT('Ctrl Pts',(4.295,2.08166817117217E-17,2.815));
#4708=CARTESIAN_POINT('Ctrl Pts',(4.295,0.0259087165500478,2.815));
#4709=CARTESIAN_POINT('Ctrl Pts',(4.3002102058406,0.0534380328956991,2.81661539166144));
#4710=CARTESIAN_POINT('Ctrl Pts',(4.32118140385364,0.103901367097065,2.82244952053683));
#4711=CARTESIAN_POINT('Ctrl Pts',(4.33693389431385,0.12684767460033,2.82659225921127));
#4712=CARTESIAN_POINT('Ctrl Pts',(4.37315766716202,0.163071447448502,2.83443540996919));
#4713=CARTESIAN_POINT('Ctrl Pts',(4.3961018032059,0.178819800999948,2.83866235487196));
#4714=CARTESIAN_POINT('Ctrl Pts',(4.4465572469413,0.199787945222222,2.84469184063064));
#4715=CARTESIAN_POINT('Ctrl Pts',(4.47408364103131,0.205,2.84639461446527));
#4716=CARTESIAN_POINT('Ctrl Pts',(4.52591635896869,0.205,2.84639461446527));
#4717=CARTESIAN_POINT('Ctrl Pts',(4.5534427530587,0.199787945222222,2.84469184063064));
#4718=CARTESIAN_POINT('Ctrl Pts',(4.6038981967941,0.178819800999948,2.83866235487196));
#4719=CARTESIAN_POINT('Ctrl Pts',(4.62684233283798,0.163071447448502,2.83443540996919));
#4720=CARTESIAN_POINT('Ctrl Pts',(4.66306610568615,0.12684767460033,2.82659225921127));
#4721=CARTESIAN_POINT('Ctrl Pts',(4.67881859614636,0.103901367097065,2.82244952053683));
#4722=CARTESIAN_POINT('Ctrl Pts',(4.6997897941594,0.0534380328956992,2.81661539166144));
#4723=CARTESIAN_POINT('Ctrl Pts',(4.705,0.0259087165500479,2.815));
#4724=CARTESIAN_POINT('Ctrl Pts',(4.705,-0.0259087165500477,2.815));
#4725=CARTESIAN_POINT('Ctrl Pts',(4.6997897941594,-0.0534380328956993,2.81661539166144));
#4726=CARTESIAN_POINT('Ctrl Pts',(4.67881859614636,-0.103901367097066,2.82244952053683));
#4727=CARTESIAN_POINT('Ctrl Pts',(4.66306610568615,-0.12684767460033,2.82659225921127));
#4728=CARTESIAN_POINT('Ctrl Pts',(4.62684233283798,-0.163071447448502,2.83443540996919));
#4729=CARTESIAN_POINT('Ctrl Pts',(4.6038981967941,-0.178819800999948,2.83866235487196));
#4730=CARTESIAN_POINT('Ctrl Pts',(4.5534427530587,-0.199787945222222,2.84469184063064));
#4731=CARTESIAN_POINT('Ctrl Pts',(4.5259163589687,-0.205,2.84639461446527));
#4732=CARTESIAN_POINT('Ctrl Pts',(4.5,-0.205,2.84639461446527));
#4733=CARTESIAN_POINT('Origin',(4.5,-1.2,1.9));
#4734=CARTESIAN_POINT('',(4.25,-1.2,2.1));
#4735=CARTESIAN_POINT('Origin',(4.5,-1.2,2.1));
#4736=CARTESIAN_POINT('',(4.25,-1.2,4.7));
#4737=CARTESIAN_POINT('',(4.25,-1.2,1.9));
#4738=CARTESIAN_POINT('Origin',(4.5,-1.2,4.7));
#4739=CARTESIAN_POINT('Origin',(4.5,-1.2,4.7));
#4740=CARTESIAN_POINT('Origin',(4.5,1.2,1.9));
#4741=CARTESIAN_POINT('',(4.25,1.2,2.1));
#4742=CARTESIAN_POINT('Origin',(4.5,1.2,2.1));
#4743=CARTESIAN_POINT('',(4.25,1.2,4.7));
#4744=CARTESIAN_POINT('',(4.25,1.2,1.9));
#4745=CARTESIAN_POINT('Origin',(4.5,1.2,4.7));
#4746=CARTESIAN_POINT('Origin',(4.5,1.2,4.7));
#4747=CARTESIAN_POINT('Origin',(4.5,-1.2,0.9));
#4748=CARTESIAN_POINT('',(4.17,-1.2,2.));
#4749=CARTESIAN_POINT('Origin',(4.5,-1.2,2.));
#4750=CARTESIAN_POINT('',(4.17,-1.2,2.1));
#4751=CARTESIAN_POINT('',(4.17,-1.2,0.9));
#4752=CARTESIAN_POINT('Origin',(4.5,-1.2,2.1));
#4753=CARTESIAN_POINT('Origin',(4.5,-1.2,2.1));
#4754=CARTESIAN_POINT('Origin',(4.5,1.2,0.9));
#4755=CARTESIAN_POINT('',(4.17,1.2,2.));
#4756=CARTESIAN_POINT('Origin',(4.5,1.2,2.));
#4757=CARTESIAN_POINT('',(4.17,1.2,2.1));
#4758=CARTESIAN_POINT('',(4.17,1.2,0.9));
#4759=CARTESIAN_POINT('Origin',(4.5,1.2,2.1));
#4760=CARTESIAN_POINT('Origin',(4.5,1.2,2.1));
#4761=CARTESIAN_POINT('Origin',(-4.5,0.,0.9));
#4762=CARTESIAN_POINT('',(-4.705,-2.51052593825207E-17,2.));
#4763=CARTESIAN_POINT('Origin',(-4.5,0.,2.));
#4764=CARTESIAN_POINT('',(-4.705,-2.98998644510284E-17,2.815));
#4765=CARTESIAN_POINT('',(-4.705,-2.51052593825207E-17,0.9));
#4766=CARTESIAN_POINT('',(-4.5,-0.205,2.84639461446527));
#4767=CARTESIAN_POINT('Ctrl Pts',(-4.5,-0.205,2.84639461446527));
#4768=CARTESIAN_POINT('Ctrl Pts',(-4.52591635896869,-0.205,2.84639461446527));
#4769=CARTESIAN_POINT('Ctrl Pts',(-4.5534427530587,-0.199787945222222,2.84469184063064));
#4770=CARTESIAN_POINT('Ctrl Pts',(-4.6038981967941,-0.178819800999948,2.83866235487196));
#4771=CARTESIAN_POINT('Ctrl Pts',(-4.62684233283798,-0.163071447448502,
2.83443540996919));
#4772=CARTESIAN_POINT('Ctrl Pts',(-4.66306610568615,-0.12684767460033,2.82659225921127));
#4773=CARTESIAN_POINT('Ctrl Pts',(-4.67881859614636,-0.103901367097065,
2.82244952053683));
#4774=CARTESIAN_POINT('Ctrl Pts',(-4.6997897941594,-0.0534380328956992,
2.81661539166144));
#4775=CARTESIAN_POINT('Ctrl Pts',(-4.705,-0.0259087165500478,2.815));
#4776=CARTESIAN_POINT('Ctrl Pts',(-4.705,-1.38777878078145E-17,2.815));
#4777=CARTESIAN_POINT('Ctrl Pts',(-4.705,-2.77555756156289E-17,2.815));
#4778=CARTESIAN_POINT('Ctrl Pts',(-4.705,0.0259087165500478,2.815));
#4779=CARTESIAN_POINT('Ctrl Pts',(-4.6997897941594,0.0534380328956991,2.81661539166144));
#4780=CARTESIAN_POINT('Ctrl Pts',(-4.67881859614636,0.103901367097065,2.82244952053683));
#4781=CARTESIAN_POINT('Ctrl Pts',(-4.66306610568615,0.12684767460033,2.82659225921127));
#4782=CARTESIAN_POINT('Ctrl Pts',(-4.62684233283798,0.163071447448502,2.83443540996919));
#4783=CARTESIAN_POINT('Ctrl Pts',(-4.6038981967941,0.178819800999948,2.83866235487196));
#4784=CARTESIAN_POINT('Ctrl Pts',(-4.5534427530587,0.199787945222222,2.84469184063064));
#4785=CARTESIAN_POINT('Ctrl Pts',(-4.52591635896869,0.205,2.84639461446527));
#4786=CARTESIAN_POINT('Ctrl Pts',(-4.47408364103131,0.205,2.84639461446527));
#4787=CARTESIAN_POINT('Ctrl Pts',(-4.4465572469413,0.199787945222222,2.84469184063064));
#4788=CARTESIAN_POINT('Ctrl Pts',(-4.3961018032059,0.178819800999948,2.83866235487196));
#4789=CARTESIAN_POINT('Ctrl Pts',(-4.37315766716202,0.163071447448502,2.83443540996919));
#4790=CARTESIAN_POINT('Ctrl Pts',(-4.33693389431385,0.12684767460033,2.82659225921127));
#4791=CARTESIAN_POINT('Ctrl Pts',(-4.32118140385364,0.103901367097065,2.82244952053683));
#4792=CARTESIAN_POINT('Ctrl Pts',(-4.3002102058406,0.0534380328956992,2.81661539166144));
#4793=CARTESIAN_POINT('Ctrl Pts',(-4.295,0.0259087165500479,2.815));
#4794=CARTESIAN_POINT('Ctrl Pts',(-4.295,-0.0259087165500477,2.815));
#4795=CARTESIAN_POINT('Ctrl Pts',(-4.3002102058406,-0.0534380328956982,
2.81661539166144));
#4796=CARTESIAN_POINT('Ctrl Pts',(-4.32118140385364,-0.103901367097065,
2.82244952053683));
#4797=CARTESIAN_POINT('Ctrl Pts',(-4.33693389431385,-0.12684767460033,2.82659225921127));
#4798=CARTESIAN_POINT('Ctrl Pts',(-4.37315766716202,-0.163071447448502,
2.83443540996919));
#4799=CARTESIAN_POINT('Ctrl Pts',(-4.3961018032059,-0.178819800999948,2.83866235487196));
#4800=CARTESIAN_POINT('Ctrl Pts',(-4.4465572469413,-0.199787945222222,2.84469184063064));
#4801=CARTESIAN_POINT('Ctrl Pts',(-4.47408364103131,-0.205,2.84639461446527));
#4802=CARTESIAN_POINT('Ctrl Pts',(-4.5,-0.205,2.84639461446527));
#4803=CARTESIAN_POINT('Origin',(-4.5,-1.2,1.9));
#4804=CARTESIAN_POINT('',(-4.75,-1.2,2.1));
#4805=CARTESIAN_POINT('Origin',(-4.5,-1.2,2.1));
#4806=CARTESIAN_POINT('',(-4.75,-1.2,4.7));
#4807=CARTESIAN_POINT('',(-4.75,-1.2,1.9));
#4808=CARTESIAN_POINT('Origin',(-4.5,-1.2,4.7));
#4809=CARTESIAN_POINT('Origin',(-4.5,-1.2,4.7));
#4810=CARTESIAN_POINT('Origin',(-4.5,1.2,1.9));
#4811=CARTESIAN_POINT('',(-4.75,1.2,2.1));
#4812=CARTESIAN_POINT('Origin',(-4.5,1.2,2.1));
#4813=CARTESIAN_POINT('',(-4.75,1.2,4.7));
#4814=CARTESIAN_POINT('',(-4.75,1.2,1.9));
#4815=CARTESIAN_POINT('Origin',(-4.5,1.2,4.7));
#4816=CARTESIAN_POINT('Origin',(-4.5,1.2,4.7));
#4817=CARTESIAN_POINT('Origin',(-4.5,-1.2,0.9));
#4818=CARTESIAN_POINT('',(-4.83,-1.2,2.));
#4819=CARTESIAN_POINT('Origin',(-4.5,-1.2,2.));
#4820=CARTESIAN_POINT('',(-4.83,-1.2,2.1));
#4821=CARTESIAN_POINT('',(-4.83,-1.2,0.9));
#4822=CARTESIAN_POINT('Origin',(-4.5,-1.2,2.1));
#4823=CARTESIAN_POINT('Origin',(-4.5,-1.2,2.1));
#4824=CARTESIAN_POINT('Origin',(-4.5,1.2,0.9));
#4825=CARTESIAN_POINT('',(-4.83,1.2,2.));
#4826=CARTESIAN_POINT('Origin',(-4.5,1.2,2.));
#4827=CARTESIAN_POINT('',(-4.83,1.2,2.1));
#4828=CARTESIAN_POINT('',(-4.83,1.2,0.9));
#4829=CARTESIAN_POINT('Origin',(-4.5,1.2,2.1));
#4830=CARTESIAN_POINT('Origin',(-4.5,1.2,2.1));
#4831=CARTESIAN_POINT('Origin',(3.75,0.,3.8));
#4832=CARTESIAN_POINT('',(-5.5,0.615812471455394,3.8));
#4833=CARTESIAN_POINT('Origin',(4.1,0.,3.5));
#4834=CARTESIAN_POINT('',(-5.5,-8.38883057415937E-17,4.185));
#4835=CARTESIAN_POINT('Origin',(-5.5,0.,3.5));
#4836=CARTESIAN_POINT('',(4.1,-8.38883057415937E-17,4.185));
#4837=CARTESIAN_POINT('',(-5.5,-0.615812471455394,3.8));
#4838=CARTESIAN_POINT('',(-1.935,-8.38883057415937E-17,4.185));
#4839=CARTESIAN_POINT('',(4.1,-8.38883057415937E-17,4.185));
#4840=CARTESIAN_POINT('',(-1.55,-0.615812471455394,3.8));
#4841=CARTESIAN_POINT('Origin',(-1.25,0.,3.5));
#4842=CARTESIAN_POINT('',(-0.95,-0.615812471455394,3.8));
#4843=CARTESIAN_POINT('',(-5.5,-0.615812471455394,3.8));
#4844=CARTESIAN_POINT('',(-0.565000000000001,-8.38883057415936E-17,4.185));
#4845=CARTESIAN_POINT('Origin',(-1.25,0.,3.5));
#4846=CARTESIAN_POINT('',(0.565000000000001,-8.38883057415936E-17,4.185));
#4847=CARTESIAN_POINT('',(4.1,-8.38883057415937E-17,4.185));
#4848=CARTESIAN_POINT('',(0.95,-0.615812471455394,3.8));
#4849=CARTESIAN_POINT('Origin',(1.25,0.,3.5));
#4850=CARTESIAN_POINT('',(1.55,-0.615812471455394,3.8));
#4851=CARTESIAN_POINT('',(-5.5,-0.615812471455394,3.8));
#4852=CARTESIAN_POINT('',(1.935,-8.38883057415936E-17,4.185));
#4853=CARTESIAN_POINT('Origin',(1.25,0.,3.5));
#4854=CARTESIAN_POINT('',(4.1,-8.38883057415937E-17,4.185));
#4855=CARTESIAN_POINT('',(5.5,8.38883057415937E-17,4.185));
#4856=CARTESIAN_POINT('',(4.1,-8.38883057415937E-17,4.185));
#4857=CARTESIAN_POINT('Origin',(5.5,0.,3.5));
#4858=CARTESIAN_POINT('Origin',(1.25,0.,3.5));
#4859=CARTESIAN_POINT('Origin',(1.25,0.,3.5));
#4860=CARTESIAN_POINT('Origin',(-1.25,0.,3.5));
#4861=CARTESIAN_POINT('Origin',(-1.25,0.,3.5));
#4862=CARTESIAN_POINT('',(-5.5,0.615812471455394,3.8));
#4863=CARTESIAN_POINT('Origin',(1.25,0.,3.8));
#4864=CARTESIAN_POINT('Origin',(1.25,0.,3.8));
#4865=CARTESIAN_POINT('Origin',(1.25,0.,3.8));
#4866=CARTESIAN_POINT('',(0.565,8.38883057415937E-17,5.));
#4867=CARTESIAN_POINT('',(0.565,-8.38883057415937E-17,3.8));
#4868=CARTESIAN_POINT('Origin',(1.25,0.,5.));
#4869=CARTESIAN_POINT('Origin',(-1.25,0.,3.8));
#4870=CARTESIAN_POINT('Origin',(-1.25,0.,3.8));
#4871=CARTESIAN_POINT('Origin',(-1.25,0.,3.8));
#4872=CARTESIAN_POINT('',(-1.935,8.38883057415937E-17,5.));
#4873=CARTESIAN_POINT('',(-1.935,-8.38883057415937E-17,3.8));
#4874=CARTESIAN_POINT('Origin',(-1.25,0.,5.));
#4875=CARTESIAN_POINT('Origin',(-3.75,0.,3.8));
#4876=CARTESIAN_POINT('Origin',(-3.75,0.,3.8));
#4877=CARTESIAN_POINT('Origin',(5.5,2.,2.));
#4878=CARTESIAN_POINT('',(5.5,2.,2.));
#4879=CARTESIAN_POINT('',(-5.5,2.,2.));
#4880=CARTESIAN_POINT('',(5.5,2.,2.));
#4881=CARTESIAN_POINT('',(-5.5,2.,5.));
#4882=CARTESIAN_POINT('',(-5.5,2.,2.));
#4883=CARTESIAN_POINT('',(5.5,2.,5.));
#4884=CARTESIAN_POINT('',(5.5,2.,5.));
#4885=CARTESIAN_POINT('',(5.5,2.,2.));
#4886=CARTESIAN_POINT('Origin',(5.5,-2.,2.));
#4887=CARTESIAN_POINT('',(5.5,-2.,2.));
#4888=CARTESIAN_POINT('',(5.5,-2.,2.));
#4889=CARTESIAN_POINT('',(5.5,-2.,5.));
#4890=CARTESIAN_POINT('',(5.5,-2.,5.));
#4891=CARTESIAN_POINT('',(5.5,-2.,2.));
#4892=CARTESIAN_POINT('Origin',(-5.5,-2.,2.));
#4893=CARTESIAN_POINT('',(-5.5,-2.,2.));
#4894=CARTESIAN_POINT('',(-5.5,-2.,2.));
#4895=CARTESIAN_POINT('',(-5.5,-2.,5.));
#4896=CARTESIAN_POINT('',(-5.5,-2.,5.));
#4897=CARTESIAN_POINT('',(-5.5,-2.,2.));
#4898=CARTESIAN_POINT('Origin',(-5.5,2.,2.));
#4899=CARTESIAN_POINT('',(-5.5,2.,2.));
#4900=CARTESIAN_POINT('',(-5.5,2.,5.));
#4901=CARTESIAN_POINT('Origin',(0.,0.,5.));
#4902=CARTESIAN_POINT('Origin',(0.,0.,2.));
#4903=CARTESIAN_POINT('',(0.,0.,0.));
#4904=CARTESIAN_POINT('Origin',(-3.75,0.,4.85));
#4905=CARTESIAN_POINT('',(-4.265,-6.30693101560887E-17,4.85));
#4906=CARTESIAN_POINT('Origin',(-3.75,0.,4.85));
#4907=CARTESIAN_POINT('',(-4.265,6.30693101560887E-17,5.5));
#4908=CARTESIAN_POINT('',(-4.265,-6.30693101560887E-17,4.85));
#4909=CARTESIAN_POINT('Origin',(-3.75,0.,5.5));
#4910=CARTESIAN_POINT('Origin',(-3.75,0.,4.85));
#4911=CARTESIAN_POINT('',(-3.95,-2.44929359829471E-17,4.85));
#4912=CARTESIAN_POINT('Origin',(-3.75,0.,4.85));
#4913=CARTESIAN_POINT('Origin',(-3.75,0.,5.));
#4914=CARTESIAN_POINT('',(-3.24481851445908,-0.875,5.));
#4915=CARTESIAN_POINT('',(-2.73963702891815,0.,5.));
#4916=CARTESIAN_POINT('',(-3.24481851445908,-0.875,5.));
#4917=CARTESIAN_POINT('',(-4.25518148554092,-0.875,5.));
#4918=CARTESIAN_POINT('',(-4.25518148554092,-0.875,5.));
#4919=CARTESIAN_POINT('',(-4.76036297108184,1.23733777851239E-16,5.));
#4920=CARTESIAN_POINT('',(-4.76036297108184,1.23733777851239E-16,5.));
#4921=CARTESIAN_POINT('',(-4.25518148554092,0.875,5.));
#4922=CARTESIAN_POINT('',(-4.25518148554092,0.875,5.));
#4923=CARTESIAN_POINT('',(-3.24481851445908,0.875,5.));
#4924=CARTESIAN_POINT('',(-3.24481851445908,0.875,5.));
#4925=CARTESIAN_POINT('',(-2.73963702891815,0.,5.));
#4926=CARTESIAN_POINT('',(-4.435,-8.38883057415937E-17,5.));
#4927=CARTESIAN_POINT('Origin',(-3.75,0.,5.));
#4928=CARTESIAN_POINT('Origin',(-4.25518148554092,-0.875,5.));
#4929=CARTESIAN_POINT('',(-3.24481851445908,-0.875,5.5));
#4930=CARTESIAN_POINT('',(-3.24481851445908,-0.875,5.));
#4931=CARTESIAN_POINT('',(-4.25518148554092,-0.875,5.5));
#4932=CARTESIAN_POINT('',(-4.25518148554092,-0.875,5.5));
#4933=CARTESIAN_POINT('',(-4.25518148554092,-0.875,5.));
#4934=CARTESIAN_POINT('Origin',(-4.76036297108184,1.23733777851239E-16,
5.));
#4935=CARTESIAN_POINT('',(-4.76036297108184,1.11022302462516E-16,5.5));
#4936=CARTESIAN_POINT('',(-4.76036297108184,1.23733777851239E-16,5.5));
#4937=CARTESIAN_POINT('',(-4.76036297108184,1.23733777851239E-16,5.));
#4938=CARTESIAN_POINT('Origin',(-4.25518148554092,0.875,5.));
#4939=CARTESIAN_POINT('',(-4.25518148554092,0.875,5.5));
#4940=CARTESIAN_POINT('',(-4.25518148554092,0.875,5.5));
#4941=CARTESIAN_POINT('',(-4.25518148554092,0.875,5.));
#4942=CARTESIAN_POINT('Origin',(-3.24481851445908,0.875,5.));
#4943=CARTESIAN_POINT('',(-3.24481851445908,0.875,5.5));
#4944=CARTESIAN_POINT('',(-3.24481851445908,0.875,5.5));
#4945=CARTESIAN_POINT('',(-3.24481851445908,0.875,5.));
#4946=CARTESIAN_POINT('Origin',(-2.73963702891815,0.,5.));
#4947=CARTESIAN_POINT('',(-2.73963702891815,0.,5.5));
#4948=CARTESIAN_POINT('',(-2.73963702891815,0.,5.5));
#4949=CARTESIAN_POINT('',(-2.73963702891815,0.,5.));
#4950=CARTESIAN_POINT('Origin',(-3.24481851445908,-0.875,5.));
#4951=CARTESIAN_POINT('',(-3.24481851445908,-0.875,5.5));
#4952=CARTESIAN_POINT('Origin',(-3.75,0.,5.5));
#4953=CARTESIAN_POINT('Origin',(-3.75,0.,3.8));
#4954=CARTESIAN_POINT('',(-3.95,-2.44929359829471E-17,3.8));
#4955=CARTESIAN_POINT('',(-3.95,-2.44929359829471E-17,3.8));
#4956=CARTESIAN_POINT('Origin',(-3.75,0.,3.8));
#4957=CARTESIAN_POINT('Origin',(-3.75,0.,3.8));
#4958=CARTESIAN_POINT('',(-4.435,-8.38883057415937E-17,3.8));
#4959=CARTESIAN_POINT('',(-4.435,-8.38883057415937E-17,3.8));
#4960=CARTESIAN_POINT('Origin',(-3.75,0.,3.8));
#4961=CARTESIAN_POINT('Origin',(-3.75,0.,3.8));
#4962=CARTESIAN_POINT('',(0.,0.,0.));
#4963=CARTESIAN_POINT('Origin',(-1.25,0.,4.85));
#4964=CARTESIAN_POINT('',(-1.765,-6.30693101560887E-17,4.85));
#4965=CARTESIAN_POINT('Origin',(-1.25,0.,4.85));
#4966=CARTESIAN_POINT('',(-1.765,6.30693101560887E-17,5.5));
#4967=CARTESIAN_POINT('',(-1.765,-6.30693101560887E-17,4.85));
#4968=CARTESIAN_POINT('Origin',(-1.25,0.,5.5));
#4969=CARTESIAN_POINT('Origin',(-1.25,0.,4.85));
#4970=CARTESIAN_POINT('',(-1.45,-2.44929359829471E-17,4.85));
#4971=CARTESIAN_POINT('Origin',(-1.25,0.,4.85));
#4972=CARTESIAN_POINT('Origin',(-1.25,0.,5.));
#4973=CARTESIAN_POINT('',(-0.744818514459077,-0.875,5.));
#4974=CARTESIAN_POINT('',(-0.239637028918155,0.,5.));
#4975=CARTESIAN_POINT('',(-0.744818514459077,-0.875,5.));
#4976=CARTESIAN_POINT('',(-1.75518148554092,-0.875,5.));
#4977=CARTESIAN_POINT('',(-1.75518148554092,-0.875,5.));
#4978=CARTESIAN_POINT('',(-2.26036297108185,1.23733777851239E-16,5.));
#4979=CARTESIAN_POINT('',(-2.26036297108185,1.23733777851239E-16,5.));
#4980=CARTESIAN_POINT('',(-1.75518148554092,0.875,5.));
#4981=CARTESIAN_POINT('',(-1.75518148554092,0.875,5.));
#4982=CARTESIAN_POINT('',(-0.744818514459077,0.875,5.));
#4983=CARTESIAN_POINT('',(-0.744818514459077,0.875,5.));
#4984=CARTESIAN_POINT('',(-0.239637028918155,0.,5.));
#4985=CARTESIAN_POINT('',(-1.935,-8.38883057415937E-17,5.));
#4986=CARTESIAN_POINT('Origin',(-1.25,0.,5.));
#4987=CARTESIAN_POINT('Origin',(-1.75518148554092,-0.875,5.));
#4988=CARTESIAN_POINT('',(-0.744818514459077,-0.875,5.5));
#4989=CARTESIAN_POINT('',(-0.744818514459077,-0.875,5.));
#4990=CARTESIAN_POINT('',(-1.75518148554092,-0.875,5.5));
#4991=CARTESIAN_POINT('',(-1.75518148554092,-0.875,5.5));
#4992=CARTESIAN_POINT('',(-1.75518148554092,-0.875,5.));
#4993=CARTESIAN_POINT('Origin',(-2.26036297108185,1.23733777851239E-16,
5.));
#4994=CARTESIAN_POINT('',(-2.26036297108185,1.11022302462516E-16,5.5));
#4995=CARTESIAN_POINT('',(-2.26036297108185,1.23733777851239E-16,5.5));
#4996=CARTESIAN_POINT('',(-2.26036297108185,1.23733777851239E-16,5.));
#4997=CARTESIAN_POINT('Origin',(-1.75518148554092,0.875,5.));
#4998=CARTESIAN_POINT('',(-1.75518148554092,0.875,5.5));
#4999=CARTESIAN_POINT('',(-1.75518148554092,0.875,5.5));
#5000=CARTESIAN_POINT('',(-1.75518148554092,0.875,5.));
#5001=CARTESIAN_POINT('Origin',(-0.744818514459077,0.875,5.));
#5002=CARTESIAN_POINT('',(-0.744818514459077,0.875,5.5));
#5003=CARTESIAN_POINT('',(-0.744818514459077,0.875,5.5));
#5004=CARTESIAN_POINT('',(-0.744818514459077,0.875,5.));
#5005=CARTESIAN_POINT('Origin',(-0.239637028918155,0.,5.));
#5006=CARTESIAN_POINT('',(-0.239637028918155,0.,5.5));
#5007=CARTESIAN_POINT('',(-0.239637028918155,0.,5.5));
#5008=CARTESIAN_POINT('',(-0.239637028918155,0.,5.));
#5009=CARTESIAN_POINT('Origin',(-0.744818514459077,-0.875,5.));
#5010=CARTESIAN_POINT('',(-0.744818514459077,-0.875,5.5));
#5011=CARTESIAN_POINT('Origin',(-1.25,0.,5.5));
#5012=CARTESIAN_POINT('Origin',(-1.25,0.,3.8));
#5013=CARTESIAN_POINT('',(-1.45,-2.44929359829471E-17,3.8));
#5014=CARTESIAN_POINT('',(-1.45,-2.44929359829471E-17,3.8));
#5015=CARTESIAN_POINT('Origin',(-1.25,0.,3.8));
#5016=CARTESIAN_POINT('Origin',(-1.25,0.,3.8));
#5017=CARTESIAN_POINT('',(-1.935,-8.38883057415937E-17,3.8));
#5018=CARTESIAN_POINT('',(-1.935,-8.38883057415937E-17,3.8));
#5019=CARTESIAN_POINT('Origin',(-1.25,0.,3.8));
#5020=CARTESIAN_POINT('Origin',(-1.25,0.,3.8));
#5021=CARTESIAN_POINT('',(0.,0.,0.));
#5022=CARTESIAN_POINT('Origin',(1.25,0.,4.85));
#5023=CARTESIAN_POINT('',(0.735,-6.30693101560887E-17,4.85));
#5024=CARTESIAN_POINT('Origin',(1.25,0.,4.85));
#5025=CARTESIAN_POINT('',(0.735,6.30693101560887E-17,5.5));
#5026=CARTESIAN_POINT('',(0.735,-6.30693101560887E-17,4.85));
#5027=CARTESIAN_POINT('Origin',(1.25,0.,5.5));
#5028=CARTESIAN_POINT('Origin',(1.25,0.,4.85));
#5029=CARTESIAN_POINT('',(1.05,-2.44929359829471E-17,4.85));
#5030=CARTESIAN_POINT('Origin',(1.25,0.,4.85));
#5031=CARTESIAN_POINT('Origin',(1.25,0.,5.));
#5032=CARTESIAN_POINT('',(1.75518148554092,-0.875,5.));
#5033=CARTESIAN_POINT('',(2.26036297108185,0.,5.));
#5034=CARTESIAN_POINT('',(1.75518148554092,-0.875,5.));
#5035=CARTESIAN_POINT('',(0.744818514459077,-0.875,5.));
#5036=CARTESIAN_POINT('',(0.744818514459077,-0.875,5.));
#5037=CARTESIAN_POINT('',(0.239637028918155,1.23733777851239E-16,5.));
#5038=CARTESIAN_POINT('',(0.239637028918155,1.23733777851239E-16,5.));
#5039=CARTESIAN_POINT('',(0.744818514459078,0.875,5.));
#5040=CARTESIAN_POINT('',(0.744818514459078,0.875,5.));
#5041=CARTESIAN_POINT('',(1.75518148554092,0.875,5.));
#5042=CARTESIAN_POINT('',(1.75518148554092,0.875,5.));
#5043=CARTESIAN_POINT('',(2.26036297108185,0.,5.));
#5044=CARTESIAN_POINT('',(0.565,-8.38883057415937E-17,5.));
#5045=CARTESIAN_POINT('Origin',(1.25,0.,5.));
#5046=CARTESIAN_POINT('Origin',(0.744818514459077,-0.875,5.));
#5047=CARTESIAN_POINT('',(1.75518148554092,-0.875,5.5));
#5048=CARTESIAN_POINT('',(1.75518148554092,-0.875,5.));
#5049=CARTESIAN_POINT('',(0.744818514459077,-0.875,5.5));
#5050=CARTESIAN_POINT('',(0.744818514459077,-0.875,5.5));
#5051=CARTESIAN_POINT('',(0.744818514459077,-0.875,5.));
#5052=CARTESIAN_POINT('Origin',(0.239637028918155,1.23733777851239E-16,
5.));
#5053=CARTESIAN_POINT('',(0.239637028918155,1.11022302462516E-16,5.5));
#5054=CARTESIAN_POINT('',(0.239637028918155,1.23733777851239E-16,5.5));
#5055=CARTESIAN_POINT('',(0.239637028918155,1.23733777851239E-16,5.));
#5056=CARTESIAN_POINT('Origin',(0.744818514459078,0.875,5.));
#5057=CARTESIAN_POINT('',(0.744818514459078,0.875,5.5));
#5058=CARTESIAN_POINT('',(0.744818514459078,0.875,5.5));
#5059=CARTESIAN_POINT('',(0.744818514459078,0.875,5.));
#5060=CARTESIAN_POINT('Origin',(1.75518148554092,0.875,5.));
#5061=CARTESIAN_POINT('',(1.75518148554092,0.875,5.5));
#5062=CARTESIAN_POINT('',(1.75518148554092,0.875,5.5));
#5063=CARTESIAN_POINT('',(1.75518148554092,0.875,5.));
#5064=CARTESIAN_POINT('Origin',(2.26036297108185,0.,5.));
#5065=CARTESIAN_POINT('',(2.26036297108185,0.,5.5));
#5066=CARTESIAN_POINT('',(2.26036297108185,0.,5.5));
#5067=CARTESIAN_POINT('',(2.26036297108185,0.,5.));
#5068=CARTESIAN_POINT('Origin',(1.75518148554092,-0.875,5.));
#5069=CARTESIAN_POINT('',(1.75518148554092,-0.875,5.5));
#5070=CARTESIAN_POINT('Origin',(1.25,0.,5.5));
#5071=CARTESIAN_POINT('Origin',(1.25,0.,3.8));
#5072=CARTESIAN_POINT('',(1.05,-2.44929359829471E-17,3.8));
#5073=CARTESIAN_POINT('',(1.05,-2.44929359829471E-17,3.8));
#5074=CARTESIAN_POINT('Origin',(1.25,0.,3.8));
#5075=CARTESIAN_POINT('Origin',(1.25,0.,3.8));
#5076=CARTESIAN_POINT('',(0.565,-8.38883057415937E-17,3.8));
#5077=CARTESIAN_POINT('',(0.565,-8.38883057415937E-17,3.8));
#5078=CARTESIAN_POINT('Origin',(1.25,0.,3.8));
#5079=CARTESIAN_POINT('Origin',(1.25,0.,3.8));
#5080=CARTESIAN_POINT('',(0.,0.,0.));
#5081=CARTESIAN_POINT('Origin',(3.75,0.,4.85));
#5082=CARTESIAN_POINT('',(3.235,-6.30693101560886E-17,4.85));
#5083=CARTESIAN_POINT('Origin',(3.75,0.,4.85));
#5084=CARTESIAN_POINT('',(3.235,6.30693101560886E-17,5.5));
#5085=CARTESIAN_POINT('',(3.235,-6.30693101560886E-17,4.85));
#5086=CARTESIAN_POINT('Origin',(3.75,0.,5.5));
#5087=CARTESIAN_POINT('Origin',(3.75,0.,4.85));
#5088=CARTESIAN_POINT('',(3.55,-2.44929359829471E-17,4.85));
#5089=CARTESIAN_POINT('Origin',(3.75,0.,4.85));
#5090=CARTESIAN_POINT('Origin',(3.75,0.,5.));
#5091=CARTESIAN_POINT('',(4.25518148554092,-0.875,5.));
#5092=CARTESIAN_POINT('',(4.76036297108184,0.,5.));
#5093=CARTESIAN_POINT('',(4.25518148554092,-0.875,5.));
#5094=CARTESIAN_POINT('',(3.24481851445908,-0.875,5.));
#5095=CARTESIAN_POINT('',(3.24481851445908,-0.875,5.));
#5096=CARTESIAN_POINT('',(2.73963702891815,1.23733777851239E-16,5.));
#5097=CARTESIAN_POINT('',(2.73963702891815,1.23733777851239E-16,5.));
#5098=CARTESIAN_POINT('',(3.24481851445908,0.875,5.));
#5099=CARTESIAN_POINT('',(3.24481851445908,0.875,5.));
#5100=CARTESIAN_POINT('',(4.25518148554092,0.875,5.));
#5101=CARTESIAN_POINT('',(4.25518148554092,0.875,5.));
#5102=CARTESIAN_POINT('',(4.76036297108184,0.,5.));
#5103=CARTESIAN_POINT('',(3.065,-8.38883057415936E-17,5.));
#5104=CARTESIAN_POINT('Origin',(3.75,0.,5.));
#5105=CARTESIAN_POINT('Origin',(3.24481851445908,-0.875,5.));
#5106=CARTESIAN_POINT('',(4.25518148554092,-0.875,5.5));
#5107=CARTESIAN_POINT('',(4.25518148554092,-0.875,5.));
#5108=CARTESIAN_POINT('',(3.24481851445908,-0.875,5.5));
#5109=CARTESIAN_POINT('',(3.24481851445908,-0.875,5.5));
#5110=CARTESIAN_POINT('',(3.24481851445908,-0.875,5.));
#5111=CARTESIAN_POINT('Origin',(2.73963702891815,1.23733777851239E-16,5.));
#5112=CARTESIAN_POINT('',(2.73963702891815,1.11022302462516E-16,5.5));
#5113=CARTESIAN_POINT('',(2.73963702891815,1.23733777851239E-16,5.5));
#5114=CARTESIAN_POINT('',(2.73963702891815,1.23733777851239E-16,5.));
#5115=CARTESIAN_POINT('Origin',(3.24481851445908,0.875,5.));
#5116=CARTESIAN_POINT('',(3.24481851445908,0.875,5.5));
#5117=CARTESIAN_POINT('',(3.24481851445908,0.875,5.5));
#5118=CARTESIAN_POINT('',(3.24481851445908,0.875,5.));
#5119=CARTESIAN_POINT('Origin',(4.25518148554092,0.875,5.));
#5120=CARTESIAN_POINT('',(4.25518148554092,0.875,5.5));
#5121=CARTESIAN_POINT('',(4.25518148554092,0.875,5.5));
#5122=CARTESIAN_POINT('',(4.25518148554092,0.875,5.));
#5123=CARTESIAN_POINT('Origin',(4.76036297108184,0.,5.));
#5124=CARTESIAN_POINT('',(4.76036297108184,0.,5.5));
#5125=CARTESIAN_POINT('',(4.76036297108184,0.,5.5));
#5126=CARTESIAN_POINT('',(4.76036297108184,0.,5.));
#5127=CARTESIAN_POINT('Origin',(4.25518148554092,-0.875,5.));
#5128=CARTESIAN_POINT('',(4.25518148554092,-0.875,5.5));
#5129=CARTESIAN_POINT('Origin',(3.75,0.,5.5));
#5130=CARTESIAN_POINT('Origin',(3.75,0.,3.8));
#5131=CARTESIAN_POINT('',(3.55,-2.44929359829471E-17,3.8));
#5132=CARTESIAN_POINT('',(3.55,-2.44929359829471E-17,3.8));
#5133=CARTESIAN_POINT('Origin',(3.75,0.,3.8));
#5134=CARTESIAN_POINT('Origin',(3.75,0.,3.8));
#5135=CARTESIAN_POINT('',(3.065,-8.38883057415936E-17,3.8));
#5136=CARTESIAN_POINT('',(3.065,-8.38883057415936E-17,3.8));
#5137=CARTESIAN_POINT('Origin',(3.75,0.,3.8));
#5138=CARTESIAN_POINT('Origin',(3.75,0.,3.8));
#5139=CARTESIAN_POINT('',(0.,0.,0.));
#5140=CARTESIAN_POINT('Origin',(-4.5,0.,0.9));
#5141=CARTESIAN_POINT('',(-4.705,-2.51052593825207E-17,1.));
#5142=CARTESIAN_POINT('Origin',(-4.5,0.,1.));
#5143=CARTESIAN_POINT('',(-4.705,2.51052593825207E-17,2.));
#5144=CARTESIAN_POINT('',(-4.705,-2.51052593825207E-17,0.9));
#5145=CARTESIAN_POINT('Origin',(-4.5,0.,2.));
#5146=CARTESIAN_POINT('Origin',(-4.5,-2.8,0.9));
#5147=CARTESIAN_POINT('',(-4.83,-2.8,1.));
#5148=CARTESIAN_POINT('Origin',(-4.5,-2.8,1.));
#5149=CARTESIAN_POINT('',(-4.83,-2.8,2.));
#5150=CARTESIAN_POINT('',(-4.83,-2.8,0.9));
#5151=CARTESIAN_POINT('Origin',(-4.5,-2.8,2.));
#5152=CARTESIAN_POINT('Origin',(-4.5,2.8,0.9));
#5153=CARTESIAN_POINT('',(-4.83,2.8,1.));
#5154=CARTESIAN_POINT('Origin',(-4.5,2.8,1.));
#5155=CARTESIAN_POINT('',(-4.83,2.8,2.));
#5156=CARTESIAN_POINT('',(-4.83,2.8,0.9));
#5157=CARTESIAN_POINT('Origin',(-4.5,2.8,2.));
#5158=CARTESIAN_POINT('Origin',(-4.5,-1.2,0.9));
#5159=CARTESIAN_POINT('',(-5.125,-1.2,1.));
#5160=CARTESIAN_POINT('Origin',(-4.5,-1.2,1.));
#5161=CARTESIAN_POINT('',(-5.125,-1.2,1.7));
#5162=CARTESIAN_POINT('',(-5.125,-1.2,0.9));
#5163=CARTESIAN_POINT('Origin',(-4.5,-1.2,1.7));
#5164=CARTESIAN_POINT('Origin',(-4.5,-1.2,1.7));
#5165=CARTESIAN_POINT('',(-4.83,-1.2,1.7));
#5166=CARTESIAN_POINT('Origin',(-4.5,-1.2,1.7));
#5167=CARTESIAN_POINT('Origin',(-4.5,1.2,0.9));
#5168=CARTESIAN_POINT('',(-5.125,1.2,1.));
#5169=CARTESIAN_POINT('Origin',(-4.5,1.2,1.));
#5170=CARTESIAN_POINT('',(-5.125,1.2,1.7));
#5171=CARTESIAN_POINT('',(-5.125,1.2,0.9));
#5172=CARTESIAN_POINT('Origin',(-4.5,1.2,1.7));
#5173=CARTESIAN_POINT('Origin',(-4.5,1.2,1.7));
#5174=CARTESIAN_POINT('',(-4.83,1.2,1.7));
#5175=CARTESIAN_POINT('Origin',(-4.5,1.2,1.7));
#5176=CARTESIAN_POINT('Origin',(-4.5,-1.2,0.9));
#5177=CARTESIAN_POINT('',(-4.83,-1.2,2.));
#5178=CARTESIAN_POINT('',(-4.83,-1.2,0.9));
#5179=CARTESIAN_POINT('Origin',(-4.5,-1.2,2.));
#5180=CARTESIAN_POINT('Origin',(-4.5,1.2,0.9));
#5181=CARTESIAN_POINT('',(-4.83,1.2,2.));
#5182=CARTESIAN_POINT('',(-4.83,1.2,0.9));
#5183=CARTESIAN_POINT('Origin',(-4.5,1.2,2.));
#5184=CARTESIAN_POINT('Origin',(-3.5,3.6,1.));
#5185=CARTESIAN_POINT('',(-3.5,3.6,1.));
#5186=CARTESIAN_POINT('',(-5.5,3.6,1.));
#5187=CARTESIAN_POINT('',(-3.5,3.6,1.));
#5188=CARTESIAN_POINT('',(-5.5,3.6,2.));
#5189=CARTESIAN_POINT('',(-5.5,3.6,1.));
#5190=CARTESIAN_POINT('',(-3.5,3.6,2.));
#5191=CARTESIAN_POINT('',(-3.5,3.6,2.));
#5192=CARTESIAN_POINT('',(-3.5,3.6,1.));
#5193=CARTESIAN_POINT('Origin',(-3.5,-3.6,1.));
#5194=CARTESIAN_POINT('',(-3.5,-3.6,1.));
#5195=CARTESIAN_POINT('',(-3.5,-3.6,1.));
#5196=CARTESIAN_POINT('',(-3.5,-3.6,2.));
#5197=CARTESIAN_POINT('',(-3.5,-3.6,2.));
#5198=CARTESIAN_POINT('',(-3.5,-3.6,1.));
#5199=CARTESIAN_POINT('Origin',(-5.5,-3.6,1.));
#5200=CARTESIAN_POINT('',(-5.5,-3.6,1.));
#5201=CARTESIAN_POINT('',(-5.5,-3.6,1.));
#5202=CARTESIAN_POINT('',(-5.5,-3.6,2.));
#5203=CARTESIAN_POINT('',(-5.5,-3.6,2.));
#5204=CARTESIAN_POINT('',(-5.5,-3.6,1.));
#5205=CARTESIAN_POINT('Origin',(-5.5,3.6,1.));
#5206=CARTESIAN_POINT('',(-5.5,3.6,1.));
#5207=CARTESIAN_POINT('',(-5.5,3.6,2.));
#5208=CARTESIAN_POINT('Origin',(-4.5,0.,2.));
#5209=CARTESIAN_POINT('Origin',(-4.5,0.,1.));
#5210=CARTESIAN_POINT('',(0.,0.,0.));
#5211=CARTESIAN_POINT('Origin',(4.5,0.,0.9));
#5212=CARTESIAN_POINT('',(4.295,-2.51052593825207E-17,1.));
#5213=CARTESIAN_POINT('Origin',(4.5,0.,1.));
#5214=CARTESIAN_POINT('',(4.295,2.51052593825207E-17,2.));
#5215=CARTESIAN_POINT('',(4.295,-2.51052593825207E-17,0.9));
#5216=CARTESIAN_POINT('Origin',(4.5,0.,2.));
#5217=CARTESIAN_POINT('Origin',(4.5,-2.8,0.9));
#5218=CARTESIAN_POINT('',(4.17,-2.8,1.));
#5219=CARTESIAN_POINT('Origin',(4.5,-2.8,1.));
#5220=CARTESIAN_POINT('',(4.17,-2.8,2.));
#5221=CARTESIAN_POINT('',(4.17,-2.8,0.9));
#5222=CARTESIAN_POINT('Origin',(4.5,-2.8,2.));
#5223=CARTESIAN_POINT('Origin',(4.5,2.8,0.9));
#5224=CARTESIAN_POINT('',(4.17,2.8,1.));
#5225=CARTESIAN_POINT('Origin',(4.5,2.8,1.));
#5226=CARTESIAN_POINT('',(4.17,2.8,2.));
#5227=CARTESIAN_POINT('',(4.17,2.8,0.9));
#5228=CARTESIAN_POINT('Origin',(4.5,2.8,2.));
#5229=CARTESIAN_POINT('Origin',(4.5,-1.2,0.9));
#5230=CARTESIAN_POINT('',(3.875,-1.2,1.));
#5231=CARTESIAN_POINT('Origin',(4.5,-1.2,1.));
#5232=CARTESIAN_POINT('',(3.875,-1.2,1.7));
#5233=CARTESIAN_POINT('',(3.875,-1.2,0.9));
#5234=CARTESIAN_POINT('Origin',(4.5,-1.2,1.7));
#5235=CARTESIAN_POINT('Origin',(4.5,-1.2,1.7));
#5236=CARTESIAN_POINT('',(4.17,-1.2,1.7));
#5237=CARTESIAN_POINT('Origin',(4.5,-1.2,1.7));
#5238=CARTESIAN_POINT('Origin',(4.5,1.2,0.9));
#5239=CARTESIAN_POINT('',(3.875,1.2,1.));
#5240=CARTESIAN_POINT('Origin',(4.5,1.2,1.));
#5241=CARTESIAN_POINT('',(3.875,1.2,1.7));
#5242=CARTESIAN_POINT('',(3.875,1.2,0.9));
#5243=CARTESIAN_POINT('Origin',(4.5,1.2,1.7));
#5244=CARTESIAN_POINT('Origin',(4.5,1.2,1.7));
#5245=CARTESIAN_POINT('',(4.17,1.2,1.7));
#5246=CARTESIAN_POINT('Origin',(4.5,1.2,1.7));
#5247=CARTESIAN_POINT('Origin',(4.5,-1.2,0.9));
#5248=CARTESIAN_POINT('',(4.17,-1.2,2.));
#5249=CARTESIAN_POINT('',(4.17,-1.2,0.9));
#5250=CARTESIAN_POINT('Origin',(4.5,-1.2,2.));
#5251=CARTESIAN_POINT('Origin',(4.5,1.2,0.9));
#5252=CARTESIAN_POINT('',(4.17,1.2,2.));
#5253=CARTESIAN_POINT('',(4.17,1.2,0.9));
#5254=CARTESIAN_POINT('Origin',(4.5,1.2,2.));
#5255=CARTESIAN_POINT('Origin',(5.5,3.6,1.));
#5256=CARTESIAN_POINT('',(5.5,3.6,1.));
#5257=CARTESIAN_POINT('',(3.5,3.6,1.));
#5258=CARTESIAN_POINT('',(5.5,3.6,1.));
#5259=CARTESIAN_POINT('',(3.5,3.6,2.));
#5260=CARTESIAN_POINT('',(3.5,3.6,1.));
#5261=CARTESIAN_POINT('',(5.5,3.6,2.));
#5262=CARTESIAN_POINT('',(5.5,3.6,2.));
#5263=CARTESIAN_POINT('',(5.5,3.6,1.));
#5264=CARTESIAN_POINT('Origin',(5.5,-3.6,1.));
#5265=CARTESIAN_POINT('',(5.5,-3.6,1.));
#5266=CARTESIAN_POINT('',(5.5,-3.6,1.));
#5267=CARTESIAN_POINT('',(5.5,-3.6,2.));
#5268=CARTESIAN_POINT('',(5.5,-3.6,2.));
#5269=CARTESIAN_POINT('',(5.5,-3.6,1.));
#5270=CARTESIAN_POINT('Origin',(3.5,-3.6,1.));
#5271=CARTESIAN_POINT('',(3.5,-3.6,1.));
#5272=CARTESIAN_POINT('',(3.5,-3.6,1.));
#5273=CARTESIAN_POINT('',(3.5,-3.6,2.));
#5274=CARTESIAN_POINT('',(3.5,-3.6,2.));
#5275=CARTESIAN_POINT('',(3.5,-3.6,1.));
#5276=CARTESIAN_POINT('Origin',(3.5,3.6,1.));
#5277=CARTESIAN_POINT('',(3.5,3.6,1.));
#5278=CARTESIAN_POINT('',(3.5,3.6,2.));
#5279=CARTESIAN_POINT('Origin',(4.5,0.,2.));
#5280=CARTESIAN_POINT('Origin',(4.5,0.,1.));
#5281=CARTESIAN_POINT('',(0.,0.,0.));
#5282=CARTESIAN_POINT('Origin',(7.91033905045424E-16,1.2,-1.33226762846206E-15));
#5283=CARTESIAN_POINT('',(-0.685,1.2,-8.38883057415937E-17));
#5284=CARTESIAN_POINT('Origin',(0.,1.2,0.));
#5285=CARTESIAN_POINT('',(-0.46,1.2,5.63337527607782E-17));
#5286=CARTESIAN_POINT('Origin',(0.,1.2,0.));
#5287=CARTESIAN_POINT('Origin',(0.,0.,0.));
#5288=CARTESIAN_POINT('',(-0.46,-1.9,-5.63337527607782E-17));
#5289=CARTESIAN_POINT('Origin',(0.,-1.9,0.));
#5290=CARTESIAN_POINT('',(-0.46,0.,-5.63337527607782E-17));
#5291=CARTESIAN_POINT('Origin',(0.,-0.4,0.));
#5292=CARTESIAN_POINT('',(1.01036297108185,-0.4,0.));
#5293=CARTESIAN_POINT('',(0.505181485540923,-0.4,0.875));
#5294=CARTESIAN_POINT('',(0.505181485540923,-0.4,0.875));
#5295=CARTESIAN_POINT('',(-0.505181485540923,-0.4,0.875));
#5296=CARTESIAN_POINT('',(-0.505181485540923,-0.4,0.875));
#5297=CARTESIAN_POINT('',(-1.01036297108185,-0.4,-1.23733777851239E-16));
#5298=CARTESIAN_POINT('',(-1.01036297108185,-0.4,-1.23733777851239E-16));
#5299=CARTESIAN_POINT('',(-0.505181485540922,-0.4,-0.875));
#5300=CARTESIAN_POINT('',(-0.505181485540922,-0.4,-0.875));
#5301=CARTESIAN_POINT('',(0.505181485540923,-0.4,-0.875));
#5302=CARTESIAN_POINT('',(0.505181485540923,-0.4,-0.875));
#5303=CARTESIAN_POINT('',(1.01036297108185,-0.4,0.));
#5304=CARTESIAN_POINT('',(-0.685,-0.4,-8.38883057415937E-17));
#5305=CARTESIAN_POINT('Origin',(0.,-0.4,0.));
#5306=CARTESIAN_POINT('Origin',(0.,0.4,0.));
#5307=CARTESIAN_POINT('',(0.505181485540923,0.4,0.875));
#5308=CARTESIAN_POINT('',(1.01036297108185,0.4,0.));
#5309=CARTESIAN_POINT('',(0.505181485540923,0.4,0.875));
#5310=CARTESIAN_POINT('',(0.505181485540923,0.4,-0.875));
#5311=CARTESIAN_POINT('',(1.01036297108185,0.4,0.));
#5312=CARTESIAN_POINT('',(-0.505181485540922,0.4,-0.875));
#5313=CARTESIAN_POINT('',(0.505181485540923,0.4,-0.875));
#5314=CARTESIAN_POINT('',(-1.01036297108185,0.4,-1.23733777851239E-16));
#5315=CARTESIAN_POINT('',(-0.505181485540922,0.4,-0.875));
#5316=CARTESIAN_POINT('',(-0.505181485540923,0.4,0.875));
#5317=CARTESIAN_POINT('',(-1.01036297108185,0.4,-1.23733777851239E-16));
#5318=CARTESIAN_POINT('',(-0.505181485540923,0.4,0.875));
#5319=CARTESIAN_POINT('',(-0.685,0.4,8.38883057415937E-17));
#5320=CARTESIAN_POINT('Origin',(0.,0.4,0.));
#5321=CARTESIAN_POINT('Origin',(-0.505181485540923,0.,0.875));
#5322=CARTESIAN_POINT('',(0.505181485540923,0.,0.875));
#5323=CARTESIAN_POINT('',(-0.505181485540923,0.,0.875));
#5324=CARTESIAN_POINT('Origin',(-1.01036297108185,0.,-1.23733777851239E-16));
#5325=CARTESIAN_POINT('',(-1.01036297108185,0.,-1.23733777851239E-16));
#5326=CARTESIAN_POINT('Origin',(-0.505181485540922,0.,-0.875));
#5327=CARTESIAN_POINT('',(-0.505181485540922,0.,-0.875));
#5328=CARTESIAN_POINT('Origin',(0.505181485540923,0.,-0.875));
#5329=CARTESIAN_POINT('',(0.505181485540923,0.,-0.875));
#5330=CARTESIAN_POINT('Origin',(1.01036297108185,0.,0.));
#5331=CARTESIAN_POINT('',(1.01036297108185,0.,0.));
#5332=CARTESIAN_POINT('Origin',(0.505181485540923,0.,0.875));
#5333=CARTESIAN_POINT('Origin',(0.,0.,0.));
#5334=CARTESIAN_POINT('',(-0.685,0.,-8.38883057415937E-17));
#5335=CARTESIAN_POINT('Origin',(0.,0.,0.));
#5336=CARTESIAN_POINT('',(-0.685,-1.82,-8.38883057415937E-17));
#5337=CARTESIAN_POINT('Origin',(0.,-1.82,0.));
#5338=CARTESIAN_POINT('',(-0.685,0.,-8.38883057415937E-17));
#5339=CARTESIAN_POINT('Origin',(0.,-1.86,0.));
#5340=CARTESIAN_POINT('',(-0.605,-1.9,-7.40911313484149E-17));
#5341=CARTESIAN_POINT('Origin',(0.,-1.9,0.));
#5342=CARTESIAN_POINT('',(-0.645,-1.86,-7.89897185450043E-17));
#5343=CARTESIAN_POINT('Origin',(0.46,-1.9,0.));
#5344=CARTESIAN_POINT('',(0.,0.,0.));
#5345=CARTESIAN_POINT('Origin',(4.1,0.,3.5));
#5346=CARTESIAN_POINT('',(5.5,-8.38883057415937E-17,4.185));
#5347=CARTESIAN_POINT('Origin',(5.5,0.,3.5));
#5348=CARTESIAN_POINT('',(5.6,-8.38883057415937E-17,4.185));
#5349=CARTESIAN_POINT('',(4.1,-8.38883057415937E-17,4.185));
#5350=CARTESIAN_POINT('Origin',(5.6,0.,3.5));
#5351=CARTESIAN_POINT('Origin',(5.6,0.,3.5));
#5352=CARTESIAN_POINT('Origin',(5.5,0.,3.5));
#5353=CARTESIAN_POINT('',(5.5,0.505181485540923,2.625));
#5354=CARTESIAN_POINT('',(5.5,1.01036297108185,3.5));
#5355=CARTESIAN_POINT('',(5.5,0.505181485540923,2.625));
#5356=CARTESIAN_POINT('',(5.5,-0.505181485540923,2.625));
#5357=CARTESIAN_POINT('',(5.5,-0.505181485540923,2.625));
#5358=CARTESIAN_POINT('',(5.5,-1.01036297108185,3.5));
#5359=CARTESIAN_POINT('',(5.5,-1.01036297108185,3.5));
#5360=CARTESIAN_POINT('',(5.5,-0.505181485540922,4.375));
#5361=CARTESIAN_POINT('',(5.5,-0.505181485540922,4.375));
#5362=CARTESIAN_POINT('',(5.5,0.505181485540923,4.375));
#5363=CARTESIAN_POINT('',(5.5,0.505181485540923,4.375));
#5364=CARTESIAN_POINT('',(5.5,1.01036297108185,3.5));
#5365=CARTESIAN_POINT('Origin',(5.5,-0.505181485540923,2.625));
#5366=CARTESIAN_POINT('',(6.1,0.505181485540923,2.625));
#5367=CARTESIAN_POINT('',(5.5,0.505181485540923,2.625));
#5368=CARTESIAN_POINT('',(6.1,-0.505181485540923,2.625));
#5369=CARTESIAN_POINT('',(6.1,-0.505181485540923,2.625));
#5370=CARTESIAN_POINT('',(5.5,-0.505181485540923,2.625));
#5371=CARTESIAN_POINT('Origin',(5.5,-1.01036297108185,3.5));
#5372=CARTESIAN_POINT('',(6.1,-1.01036297108185,3.5));
#5373=CARTESIAN_POINT('',(6.1,-1.01036297108185,3.5));
#5374=CARTESIAN_POINT('',(5.5,-1.01036297108185,3.5));
#5375=CARTESIAN_POINT('Origin',(5.5,-0.505181485540922,4.375));
#5376=CARTESIAN_POINT('',(6.1,-0.505181485540922,4.375));
#5377=CARTESIAN_POINT('',(6.1,-0.505181485540922,4.375));
#5378=CARTESIAN_POINT('',(5.5,-0.505181485540922,4.375));
#5379=CARTESIAN_POINT('Origin',(5.5,0.505181485540923,4.375));
#5380=CARTESIAN_POINT('',(6.1,0.505181485540923,4.375));
#5381=CARTESIAN_POINT('',(6.1,0.505181485540923,4.375));
#5382=CARTESIAN_POINT('',(5.5,0.505181485540923,4.375));
#5383=CARTESIAN_POINT('Origin',(5.5,1.01036297108185,3.5));
#5384=CARTESIAN_POINT('',(6.1,1.01036297108185,3.5));
#5385=CARTESIAN_POINT('',(6.1,1.01036297108185,3.5));
#5386=CARTESIAN_POINT('',(5.5,1.01036297108185,3.5));
#5387=CARTESIAN_POINT('Origin',(5.5,0.505181485540923,2.625));
#5388=CARTESIAN_POINT('',(6.1,0.505181485540923,2.625));
#5389=CARTESIAN_POINT('Origin',(6.1,0.,3.5));
#5390=CARTESIAN_POINT('',(0.,0.,0.));
#5391=CARTESIAN_POINT('',(0.,0.,0.));
#5392=CARTESIAN_POINT('Origin',(0.,0.6,0.));
#5393=CARTESIAN_POINT('',(-0.43,0.6,5.26598123633362E-17));
#5394=CARTESIAN_POINT('Origin',(0.,0.6,0.));
#5395=CARTESIAN_POINT('',(-0.43,0.7,-5.26598123633362E-17));
#5396=CARTESIAN_POINT('',(-0.43,0.6,5.26598123633362E-17));
#5397=CARTESIAN_POINT('Origin',(0.,0.7,0.));
#5398=CARTESIAN_POINT('Origin',(0.,0.6,0.));
#5399=CARTESIAN_POINT('',(-0.2,0.6,2.44929359829471E-17));
#5400=CARTESIAN_POINT('Origin',(0.,0.6,0.));
#5401=CARTESIAN_POINT('Origin',(0.,0.5,-1.11022302462516E-16));
#5402=CARTESIAN_POINT('',(0.346410161513776,0.5,0.6));
#5403=CARTESIAN_POINT('',(0.692820323027551,0.5,0.));
#5404=CARTESIAN_POINT('',(0.346410161513776,0.5,0.6));
#5405=CARTESIAN_POINT('',(0.346410161513776,0.5,-0.6));
#5406=CARTESIAN_POINT('',(0.692820323027551,0.5,0.));
#5407=CARTESIAN_POINT('',(-0.346410161513775,0.5,-0.6));
#5408=CARTESIAN_POINT('',(0.346410161513776,0.5,-0.6));
#5409=CARTESIAN_POINT('',(-0.692820323027551,0.5,-8.48460190979926E-17));
#5410=CARTESIAN_POINT('',(-0.346410161513775,0.5,-0.6));
#5411=CARTESIAN_POINT('',(-0.346410161513776,0.5,0.6));
#5412=CARTESIAN_POINT('',(-0.692820323027551,0.5,-8.48460190979926E-17));
#5413=CARTESIAN_POINT('',(-0.346410161513776,0.5,0.6));
#5414=CARTESIAN_POINT('',(-0.525,0.5,-6.4293956955236E-17));
#5415=CARTESIAN_POINT('Origin',(0.,0.5,0.));
#5416=CARTESIAN_POINT('Origin',(0.,0.,-1.11022302462516E-16));
#5417=CARTESIAN_POINT('',(0.346410161513776,0.,0.6));
#5418=CARTESIAN_POINT('',(0.692820323027551,0.,0.));
#5419=CARTESIAN_POINT('',(0.346410161513776,0.,0.6));
#5420=CARTESIAN_POINT('',(-0.346410161513776,0.,0.6));
#5421=CARTESIAN_POINT('',(-0.346410161513776,0.,0.6));
#5422=CARTESIAN_POINT('',(-0.692820323027551,0.,-8.48460190979926E-17));
#5423=CARTESIAN_POINT('',(-0.692820323027551,0.,-8.48460190979926E-17));
#5424=CARTESIAN_POINT('',(-0.346410161513775,0.,-0.6));
#5425=CARTESIAN_POINT('',(-0.346410161513775,0.,-0.6));
#5426=CARTESIAN_POINT('',(0.346410161513776,0.,-0.6));
#5427=CARTESIAN_POINT('',(0.346410161513776,0.,-0.6));
#5428=CARTESIAN_POINT('',(0.692820323027551,0.,0.));
#5429=CARTESIAN_POINT('',(-0.515,0.,-6.30693101560887E-17));
#5430=CARTESIAN_POINT('Origin',(0.,0.,0.));
#5431=CARTESIAN_POINT('Origin',(-0.346410161513776,0.,0.6));
#5432=CARTESIAN_POINT('',(0.346410161513776,0.,0.6));
#5433=CARTESIAN_POINT('',(-0.346410161513776,0.,0.6));
#5434=CARTESIAN_POINT('Origin',(-0.692820323027551,0.,-8.48460190979926E-17));
#5435=CARTESIAN_POINT('',(-0.692820323027551,0.,-8.48460190979926E-17));
#5436=CARTESIAN_POINT('Origin',(-0.346410161513775,0.,-0.6));
#5437=CARTESIAN_POINT('',(-0.346410161513775,0.,-0.6));
#5438=CARTESIAN_POINT('Origin',(0.346410161513776,0.,-0.6));
#5439=CARTESIAN_POINT('',(0.346410161513776,0.,-0.6));
#5440=CARTESIAN_POINT('Origin',(0.692820323027551,0.,0.));
#5441=CARTESIAN_POINT('',(0.692820323027551,0.,0.));
#5442=CARTESIAN_POINT('Origin',(0.346410161513776,0.,0.6));
#5443=CARTESIAN_POINT('Origin',(0.46,0.7,0.));
#5444=CARTESIAN_POINT('',(-0.46,0.7,-5.63337527607782E-17));
#5445=CARTESIAN_POINT('Origin',(0.,0.7,0.));
#5446=CARTESIAN_POINT('Origin',(0.,1.2,0.));
#5447=CARTESIAN_POINT('',(-0.46,1.7,-5.63337527607782E-17));
#5448=CARTESIAN_POINT('',(-0.46,1.2,-5.63337527607782E-17));
#5449=CARTESIAN_POINT('Origin',(0.,1.7,0.));
#5450=CARTESIAN_POINT('Origin',(0.525,1.7,0.));
#5451=CARTESIAN_POINT('',(-0.525,1.7,-6.4293956955236E-17));
#5452=CARTESIAN_POINT('Origin',(0.,1.7,0.));
#5453=CARTESIAN_POINT('Origin',(0.,1.1,0.));
#5454=CARTESIAN_POINT('',(-0.525,1.1,-6.4293956955236E-17));
#5455=CARTESIAN_POINT('Origin',(0.,-0.325,0.));
#5456=CARTESIAN_POINT('',(-0.515,-0.65,-6.30693101560887E-17));
#5457=CARTESIAN_POINT('Origin',(0.,-0.65,0.));
#5458=CARTESIAN_POINT('',(-0.515,-0.325,-6.30693101560887E-17));
#5459=CARTESIAN_POINT('Origin',(0.2,-0.65,0.));
#5460=CARTESIAN_POINT('',(-0.2,-0.65,-2.44929359829471E-17));
#5461=CARTESIAN_POINT('Origin',(0.,-0.65,0.));
#5462=CARTESIAN_POINT('Origin',(0.,0.0249999999999999,0.));
#5463=CARTESIAN_POINT('',(-0.2,0.0249999999999999,-2.44929359829471E-17));
#5464=CARTESIAN_POINT('',(0.,0.,0.));
#5465=CARTESIAN_POINT('Origin',(0.475,1.95,0.));
#5466=CARTESIAN_POINT('',(-0.475,1.95,-5.81707229594993E-17));
#5467=CARTESIAN_POINT('Origin',(0.,1.95,0.));
#5468=CARTESIAN_POINT('',(-0.31,1.95,-3.7964050773568E-17));
#5469=CARTESIAN_POINT('Origin',(0.,1.95,0.));
#5470=CARTESIAN_POINT('Origin',(0.,1.825,0.));
#5471=CARTESIAN_POINT('',(-0.475,1.7,-5.81707229594993E-17));
#5472=CARTESIAN_POINT('Origin',(0.,1.7,0.));
#5473=CARTESIAN_POINT('',(-0.475,1.825,-5.81707229594993E-17));
#5474=CARTESIAN_POINT('Origin',(0.355,1.7,0.));
#5475=CARTESIAN_POINT('',(-0.355,1.7,-4.3474961369731E-17));
#5476=CARTESIAN_POINT('Origin',(0.,1.7,0.));
#5477=CARTESIAN_POINT('Origin',(0.,1.55,0.));
#5478=CARTESIAN_POINT('',(-0.355,1.4,-4.3474961369731E-17));
#5479=CARTESIAN_POINT('Origin',(0.,1.4,0.));
#5480=CARTESIAN_POINT('',(-0.355,1.55,-4.3474961369731E-17));
#5481=CARTESIAN_POINT('Origin',(0.31,1.4,0.));
#5482=CARTESIAN_POINT('',(-0.31,1.4,-3.7964050773568E-17));
#5483=CARTESIAN_POINT('Origin',(0.,1.4,0.));
#5484=CARTESIAN_POINT('Origin',(0.,1.675,0.));
#5485=CARTESIAN_POINT('',(-0.31,1.675,-3.7964050773568E-17));
#5486=CARTESIAN_POINT('',(0.,0.,0.));
#5487=CARTESIAN_POINT('',(0.,0.,0.));
#5488=CARTESIAN_POINT('',(0.,0.,0.));
#5489=CARTESIAN_POINT('Origin',(1.42247325030098E-15,1.60000000000001,0.));
#5490=CARTESIAN_POINT('',(-0.2,1.94641016151378,-2.44929359829471E-17));
#5491=CARTESIAN_POINT('Origin',(0.,1.94641016151378,0.));
#5492=CARTESIAN_POINT('Origin',(0.,1.00320508075689,0.));
#5493=CARTESIAN_POINT('',(-0.2,0.0600000000000001,-2.44929359829471E-17));
#5494=CARTESIAN_POINT('Origin',(0.,0.06,0.));
#5495=CARTESIAN_POINT('',(-0.2,1.00320508075689,-2.44929359829471E-17));
#5496=CARTESIAN_POINT('Origin',(0.,0.03,0.));
#5497=CARTESIAN_POINT('',(-0.14,3.46944695195361E-18,-1.71450551880629E-17));
#5498=CARTESIAN_POINT('Origin',(0.,0.,0.));
#5499=CARTESIAN_POINT('',(-0.17,0.03,-2.0818995585505E-17));
#5500=CARTESIAN_POINT('Origin',(0.,0.,0.));
#5501=CARTESIAN_POINT('',(0.,0.,0.));
#5502=CARTESIAN_POINT('Origin',(0.,0.,0.));
#5503=CARTESIAN_POINT('',(-0.32,0.16,3.91886975727153E-17));
#5504=CARTESIAN_POINT('Origin',(0.,0.16,0.));
#5505=CARTESIAN_POINT('',(-0.32,0.,3.91886975727153E-17));
#5506=CARTESIAN_POINT('',(-0.32,0.,3.91886975727153E-17));
#5507=CARTESIAN_POINT('Origin',(0.,0.,0.));
#5508=CARTESIAN_POINT('Origin',(0.,0.,0.));
#5509=CARTESIAN_POINT('',(-0.6,0.16,7.34788079488412E-17));
#5510=CARTESIAN_POINT('Origin',(0.,0.16,0.));
#5511=CARTESIAN_POINT('',(-0.6,0.,7.34788079488412E-17));
#5512=CARTESIAN_POINT('',(-0.6,0.,7.34788079488412E-17));
#5513=CARTESIAN_POINT('Origin',(0.,0.,0.));
#5514=CARTESIAN_POINT('Origin',(0.,0.16,0.));
#5515=CARTESIAN_POINT('Origin',(0.,0.,0.));
#5516=CARTESIAN_POINT('',(0.,0.,0.));
#5517=CARTESIAN_POINT('Origin',(0.,-1.445,0.));
#5518=CARTESIAN_POINT('',(-0.2942,-2.9458,3.60291088309151E-17));
#5519=CARTESIAN_POINT('Origin',(0.,-2.9458,0.));
#5520=CARTESIAN_POINT('',(-0.2942,0.,-3.60291088309151E-17));
#5521=CARTESIAN_POINT('',(-0.2942,-1.445,-3.60291088309151E-17));
#5522=CARTESIAN_POINT('Origin',(0.,0.,0.));
#5523=CARTESIAN_POINT('Origin',(0.,-2.97,0.));
#5524=CARTESIAN_POINT('',(-0.24,-3.,-2.93915231795365E-17));
#5525=CARTESIAN_POINT('Origin',(0.,-3.,0.));
#5526=CARTESIAN_POINT('',(-0.27,-2.97,-3.30654635769785E-17));
#5527=CARTESIAN_POINT('Origin',(0.,-3.,0.));
#5528=CARTESIAN_POINT('Origin',(0.,0.341586508806388,0.));
#5529=CARTESIAN_POINT('',(-0.475,0.4,-5.81707229594993E-17));
#5530=CARTESIAN_POINT('Origin',(0.,0.4,0.));
#5531=CARTESIAN_POINT('',(-0.577350269189626,0.340908044531739,-7.07050159149938E-17));
#5532=CARTESIAN_POINT('',(-0.576175134594813,0.341586508806388,-7.05611034329833E-17));
#5533=CARTESIAN_POINT('',(-0.288675134594813,0.340908044531739,0.5));
#5534=CARTESIAN_POINT('Ctrl Pts',(-0.288675134594813,0.340908044531739,
0.5));
#5535=CARTESIAN_POINT('Ctrl Pts',(-0.433012701893303,0.424241377863696,
0.249999999998124));
#5536=CARTESIAN_POINT('Ctrl Pts',(-0.577350269189626,0.340908044531739,
-7.07050159149938E-17));
#5537=CARTESIAN_POINT('',(0.288675134594813,0.340908044531739,0.5));
#5538=CARTESIAN_POINT('Ctrl Pts',(0.288675134594813,0.340908044531739,0.5));
#5539=CARTESIAN_POINT('Ctrl Pts',(-2.16648921025353E-12,0.424241377863696,
0.5));
#5540=CARTESIAN_POINT('Ctrl Pts',(-0.288675134594813,0.340908044531739,
0.5));
#5541=CARTESIAN_POINT('',(0.577350269189626,0.340908044531739,0.));
#5542=CARTESIAN_POINT('Ctrl Pts',(0.577350269189626,0.340908044531739,0.));
#5543=CARTESIAN_POINT('Ctrl Pts',(0.433012701891136,0.424241377863697,0.250000000001876));
#5544=CARTESIAN_POINT('Ctrl Pts',(0.288675134594813,0.340908044531739,0.5));
#5545=CARTESIAN_POINT('',(0.288675134594813,0.340908044531739,-0.5));
#5546=CARTESIAN_POINT('Ctrl Pts',(0.288675134594813,0.340908044531739,-0.5));
#5547=CARTESIAN_POINT('Ctrl Pts',(0.433012701893303,0.424241377863696,-0.249999999998124));
#5548=CARTESIAN_POINT('Ctrl Pts',(0.577350269189626,0.340908044531739,0.));
#5549=CARTESIAN_POINT('',(-0.288675134594813,0.340908044531739,-0.5));
#5550=CARTESIAN_POINT('Ctrl Pts',(-0.288675134594813,0.340908044531739,
-0.5));
#5551=CARTESIAN_POINT('Ctrl Pts',(2.16660023255599E-12,0.424241377863696,
-0.5));
#5552=CARTESIAN_POINT('Ctrl Pts',(0.288675134594813,0.340908044531739,-0.5));
#5553=CARTESIAN_POINT('Ctrl Pts',(-0.577350269189626,0.340908044531739,
-7.07050159149938E-17));
#5554=CARTESIAN_POINT('Ctrl Pts',(-0.433012701891136,0.424241377863697,
-0.250000000001876));
#5555=CARTESIAN_POINT('Ctrl Pts',(-0.288675134594813,0.340908044531739,
-0.5));
#5556=CARTESIAN_POINT('Origin',(0.288675134594813,0.,-0.5));
#5557=CARTESIAN_POINT('',(0.288675134594813,0.,-0.5));
#5558=CARTESIAN_POINT('',(0.288675134594813,0.,-0.5));
#5559=CARTESIAN_POINT('',(-0.288675134594813,0.,-0.5));
#5560=CARTESIAN_POINT('',(0.288675134594813,0.,-0.5));
#5561=CARTESIAN_POINT('',(-0.288675134594813,0.,-0.5));
#5562=CARTESIAN_POINT('Origin',(0.577350269189626,0.,0.));
#5563=CARTESIAN_POINT('',(0.577350269189626,0.,0.));
#5564=CARTESIAN_POINT('',(0.577350269189626,0.,0.));
#5565=CARTESIAN_POINT('',(0.577350269189626,0.,0.));
#5566=CARTESIAN_POINT('Origin',(0.288675134594813,0.,0.5));
#5567=CARTESIAN_POINT('',(0.288675134594813,0.,0.5));
#5568=CARTESIAN_POINT('',(0.288675134594813,0.,0.5));
#5569=CARTESIAN_POINT('',(0.288675134594813,0.,0.5));
#5570=CARTESIAN_POINT('Origin',(-0.288675134594813,0.,0.5));
#5571=CARTESIAN_POINT('',(-0.288675134594813,0.,0.5));
#5572=CARTESIAN_POINT('',(-0.288675134594813,0.,0.5));
#5573=CARTESIAN_POINT('',(-0.288675134594813,0.,0.5));
#5574=CARTESIAN_POINT('Origin',(-0.577350269189626,0.,-7.07050159149938E-17));
#5575=CARTESIAN_POINT('',(-0.577350269189626,0.,-7.07050159149938E-17));
#5576=CARTESIAN_POINT('',(-0.577350269189626,0.,-7.07050159149938E-17));
#5577=CARTESIAN_POINT('',(-0.577350269189626,0.,-7.07050159149938E-17));
#5578=CARTESIAN_POINT('Origin',(-0.288675134594813,0.,-0.5));
#5579=CARTESIAN_POINT('',(-0.288675134594813,0.,-0.5));
#5580=CARTESIAN_POINT('Origin',(0.,0.4,0.));
#5581=CARTESIAN_POINT('Origin',(0.,0.,0.));
#5582=CARTESIAN_POINT('',(0.,0.,0.));
#5583=CARTESIAN_POINT('',(0.,0.,0.));
#5584=CARTESIAN_POINT('',(0.,0.,0.));
#5585=CARTESIAN_POINT('',(0.,0.,0.));
#5586=CARTESIAN_POINT('',(0.,0.,0.));
#5587=CARTESIAN_POINT('',(0.,0.,0.));
#5588=CARTESIAN_POINT('',(0.,0.,0.));
#5589=CARTESIAN_POINT('',(-5.9,-1.38777878078145E-17,3.5));
#5590=CARTESIAN_POINT('',(0.,0.,0.));
#5591=CARTESIAN_POINT('',(-3.75,0.,5.5));
#5592=CARTESIAN_POINT('',(-1.25,0.,5.5));
#5593=CARTESIAN_POINT('',(1.25,0.,5.5));
#5594=CARTESIAN_POINT('',(3.75,0.,5.5));
#5595=CARTESIAN_POINT('',(-4.5,0.,1.));
#5596=CARTESIAN_POINT('',(-4.5,-1.2,1.7));
#5597=CARTESIAN_POINT('',(-4.5,-1.2,1.54));
#5598=CARTESIAN_POINT('',(-4.5,1.2,1.7));
#5599=CARTESIAN_POINT('',(-4.5,1.2,1.54));
#5600=CARTESIAN_POINT('',(4.5,0.,1.));
#5601=CARTESIAN_POINT('',(4.5,-1.2,1.7));
#5602=CARTESIAN_POINT('',(4.5,-1.2,1.54));
#5603=CARTESIAN_POINT('',(4.5,1.2,1.7));
#5604=CARTESIAN_POINT('',(4.5,1.2,1.54));
#5605=UNCERTAINTY_MEASURE_WITH_UNIT(LENGTH_MEASURE(0.001),#5639,
'DISTANCE_ACCURACY_VALUE',
'Maximum model space distance between geometric entities at asserted c
onnectivities');
#5606=UNCERTAINTY_MEASURE_WITH_UNIT(LENGTH_MEASURE(0.001),#5639,
'DISTANCE_ACCURACY_VALUE',
'Maximum model space distance between geometric entities at asserted c
onnectivities');
#5607=UNCERTAINTY_MEASURE_WITH_UNIT(LENGTH_MEASURE(0.001),#5639,
'DISTANCE_ACCURACY_VALUE',
'Maximum model space distance between geometric entities at asserted c
onnectivities');
#5608=UNCERTAINTY_MEASURE_WITH_UNIT(LENGTH_MEASURE(0.001),#5639,
'DISTANCE_ACCURACY_VALUE',
'Maximum model space distance between geometric entities at asserted c
onnectivities');
#5609=UNCERTAINTY_MEASURE_WITH_UNIT(LENGTH_MEASURE(0.001),#5639,
'DISTANCE_ACCURACY_VALUE',
'Maximum model space distance between geometric entities at asserted c
onnectivities');
#5610=UNCERTAINTY_MEASURE_WITH_UNIT(LENGTH_MEASURE(0.001),#5639,
'DISTANCE_ACCURACY_VALUE',
'Maximum model space distance between geometric entities at asserted c
onnectivities');
#5611=UNCERTAINTY_MEASURE_WITH_UNIT(LENGTH_MEASURE(0.001),#5639,
'DISTANCE_ACCURACY_VALUE',
'Maximum model space distance between geometric entities at asserted c
onnectivities');
#5612=UNCERTAINTY_MEASURE_WITH_UNIT(LENGTH_MEASURE(0.001),#5639,
'DISTANCE_ACCURACY_VALUE',
'Maximum model space distance between geometric entities at asserted c
onnectivities');
#5613=UNCERTAINTY_MEASURE_WITH_UNIT(LENGTH_MEASURE(0.001),#5639,
'DISTANCE_ACCURACY_VALUE',
'Maximum model space distance between geometric entities at asserted c
onnectivities');
#5614=UNCERTAINTY_MEASURE_WITH_UNIT(LENGTH_MEASURE(0.001),#5639,
'DISTANCE_ACCURACY_VALUE',
'Maximum model space distance between geometric entities at asserted c
onnectivities');
#5615=UNCERTAINTY_MEASURE_WITH_UNIT(LENGTH_MEASURE(0.001),#5639,
'DISTANCE_ACCURACY_VALUE',
'Maximum model space distance between geometric entities at asserted c
onnectivities');
#5616=UNCERTAINTY_MEASURE_WITH_UNIT(LENGTH_MEASURE(0.001),#5639,
'DISTANCE_ACCURACY_VALUE',
'Maximum model space distance between geometric entities at asserted c
onnectivities');
#5617=UNCERTAINTY_MEASURE_WITH_UNIT(LENGTH_MEASURE(0.001),#5639,
'DISTANCE_ACCURACY_VALUE',
'Maximum model space distance between geometric entities at asserted c
onnectivities');
#5618=UNCERTAINTY_MEASURE_WITH_UNIT(LENGTH_MEASURE(0.001),#5639,
'DISTANCE_ACCURACY_VALUE',
'Maximum model space distance between geometric entities at asserted c
onnectivities');
#5619=UNCERTAINTY_MEASURE_WITH_UNIT(LENGTH_MEASURE(0.001),#5639,
'DISTANCE_ACCURACY_VALUE',
'Maximum model space distance between geometric entities at asserted c
onnectivities');
#5620=UNCERTAINTY_MEASURE_WITH_UNIT(LENGTH_MEASURE(0.001),#5639,
'DISTANCE_ACCURACY_VALUE',
'Maximum model space distance between geometric entities at asserted c
onnectivities');
#5621=UNCERTAINTY_MEASURE_WITH_UNIT(LENGTH_MEASURE(0.001),#5639,
'DISTANCE_ACCURACY_VALUE',
'Maximum model space distance between geometric entities at asserted c
onnectivities');
#5622=(
GEOMETRIC_REPRESENTATION_CONTEXT(3)
GLOBAL_UNCERTAINTY_ASSIGNED_CONTEXT((#5605))
GLOBAL_UNIT_ASSIGNED_CONTEXT((#5639,#5641,#5642))
REPRESENTATION_CONTEXT('','3D')
);
#5623=(
GEOMETRIC_REPRESENTATION_CONTEXT(3)
GLOBAL_UNCERTAINTY_ASSIGNED_CONTEXT((#5606))
GLOBAL_UNIT_ASSIGNED_CONTEXT((#5639,#5641,#5642))
REPRESENTATION_CONTEXT('','3D')
);
#5624=(
GEOMETRIC_REPRESENTATION_CONTEXT(3)
GLOBAL_UNCERTAINTY_ASSIGNED_CONTEXT((#5607))
GLOBAL_UNIT_ASSIGNED_CONTEXT((#5639,#5641,#5642))
REPRESENTATION_CONTEXT('','3D')
);
#5625=(
GEOMETRIC_REPRESENTATION_CONTEXT(3)
GLOBAL_UNCERTAINTY_ASSIGNED_CONTEXT((#5608))
GLOBAL_UNIT_ASSIGNED_CONTEXT((#5639,#5641,#5642))
REPRESENTATION_CONTEXT('','3D')
);
#5626=(
GEOMETRIC_REPRESENTATION_CONTEXT(3)
GLOBAL_UNCERTAINTY_ASSIGNED_CONTEXT((#5609))
GLOBAL_UNIT_ASSIGNED_CONTEXT((#5639,#5641,#5642))
REPRESENTATION_CONTEXT('','3D')
);
#5627=(
GEOMETRIC_REPRESENTATION_CONTEXT(3)
GLOBAL_UNCERTAINTY_ASSIGNED_CONTEXT((#5610))
GLOBAL_UNIT_ASSIGNED_CONTEXT((#5639,#5641,#5642))
REPRESENTATION_CONTEXT('','3D')
);
#5628=(
GEOMETRIC_REPRESENTATION_CONTEXT(3)
GLOBAL_UNCERTAINTY_ASSIGNED_CONTEXT((#5611))
GLOBAL_UNIT_ASSIGNED_CONTEXT((#5639,#5641,#5642))
REPRESENTATION_CONTEXT('','3D')
);
#5629=(
GEOMETRIC_REPRESENTATION_CONTEXT(3)
GLOBAL_UNCERTAINTY_ASSIGNED_CONTEXT((#5612))
GLOBAL_UNIT_ASSIGNED_CONTEXT((#5639,#5641,#5642))
REPRESENTATION_CONTEXT('','3D')
);
#5630=(
GEOMETRIC_REPRESENTATION_CONTEXT(3)
GLOBAL_UNCERTAINTY_ASSIGNED_CONTEXT((#5613))
GLOBAL_UNIT_ASSIGNED_CONTEXT((#5639,#5641,#5642))
REPRESENTATION_CONTEXT('','3D')
);
#5631=(
GEOMETRIC_REPRESENTATION_CONTEXT(3)
GLOBAL_UNCERTAINTY_ASSIGNED_CONTEXT((#5614))
GLOBAL_UNIT_ASSIGNED_CONTEXT((#5639,#5641,#5642))
REPRESENTATION_CONTEXT('','3D')
);
#5632=(
GEOMETRIC_REPRESENTATION_CONTEXT(3)
GLOBAL_UNCERTAINTY_ASSIGNED_CONTEXT((#5615))
GLOBAL_UNIT_ASSIGNED_CONTEXT((#5639,#5641,#5642))
REPRESENTATION_CONTEXT('','3D')
);
#5633=(
GEOMETRIC_REPRESENTATION_CONTEXT(3)
GLOBAL_UNCERTAINTY_ASSIGNED_CONTEXT((#5616))
GLOBAL_UNIT_ASSIGNED_CONTEXT((#5639,#5641,#5642))
REPRESENTATION_CONTEXT('','3D')
);
#5634=(
GEOMETRIC_REPRESENTATION_CONTEXT(3)
GLOBAL_UNCERTAINTY_ASSIGNED_CONTEXT((#5617))
GLOBAL_UNIT_ASSIGNED_CONTEXT((#5639,#5641,#5642))
REPRESENTATION_CONTEXT('','3D')
);
#5635=(
GEOMETRIC_REPRESENTATION_CONTEXT(3)
GLOBAL_UNCERTAINTY_ASSIGNED_CONTEXT((#5618))
GLOBAL_UNIT_ASSIGNED_CONTEXT((#5639,#5641,#5642))
REPRESENTATION_CONTEXT('','3D')
);
#5636=(
GEOMETRIC_REPRESENTATION_CONTEXT(3)
GLOBAL_UNCERTAINTY_ASSIGNED_CONTEXT((#5619))
GLOBAL_UNIT_ASSIGNED_CONTEXT((#5639,#5641,#5642))
REPRESENTATION_CONTEXT('','3D')
);
#5637=(
GEOMETRIC_REPRESENTATION_CONTEXT(3)
GLOBAL_UNCERTAINTY_ASSIGNED_CONTEXT((#5620))
GLOBAL_UNIT_ASSIGNED_CONTEXT((#5639,#5641,#5642))
REPRESENTATION_CONTEXT('','3D')
);
#5638=(
GEOMETRIC_REPRESENTATION_CONTEXT(3)
GLOBAL_UNCERTAINTY_ASSIGNED_CONTEXT((#5621))
GLOBAL_UNIT_ASSIGNED_CONTEXT((#5639,#5641,#5642))
REPRESENTATION_CONTEXT('','3D')
);
#5639=(
LENGTH_UNIT()
NAMED_UNIT(*)
SI_UNIT(.CENTI.,.METRE.)
);
#5640=(
LENGTH_UNIT()
NAMED_UNIT(*)
SI_UNIT($,.METRE.)
);
#5641=(
NAMED_UNIT(*)
PLANE_ANGLE_UNIT()
SI_UNIT($,.RADIAN.)
);
#5642=(
NAMED_UNIT(*)
SI_UNIT($,.STERADIAN.)
SOLID_ANGLE_UNIT()
);
#5643=SHAPE_DEFINITION_REPRESENTATION(#5659,#5700);
#5644=SHAPE_DEFINITION_REPRESENTATION(#5660,#5701);
#5645=SHAPE_DEFINITION_REPRESENTATION(#5661,#5702);
#5646=SHAPE_DEFINITION_REPRESENTATION(#5662,#5703);
#5647=SHAPE_DEFINITION_REPRESENTATION(#5663,#5704);
#5648=SHAPE_DEFINITION_REPRESENTATION(#5664,#5705);
#5649=SHAPE_DEFINITION_REPRESENTATION(#5665,#5706);
#5650=SHAPE_DEFINITION_REPRESENTATION(#5666,#5707);
#5651=SHAPE_DEFINITION_REPRESENTATION(#5667,#5708);
#5652=SHAPE_DEFINITION_REPRESENTATION(#5668,#5709);
#5653=SHAPE_DEFINITION_REPRESENTATION(#5669,#5710);
#5654=SHAPE_DEFINITION_REPRESENTATION(#5670,#5711);
#5655=SHAPE_DEFINITION_REPRESENTATION(#5671,#5712);
#5656=SHAPE_DEFINITION_REPRESENTATION(#5674,#5713);
#5657=SHAPE_DEFINITION_REPRESENTATION(#5675,#5714);
#5658=SHAPE_DEFINITION_REPRESENTATION(#5676,#5715);
#5659=PRODUCT_DEFINITION_SHAPE('',$,#5717);
#5660=PRODUCT_DEFINITION_SHAPE('',$,#5718);
#5661=PRODUCT_DEFINITION_SHAPE('',$,#5719);
#5662=PRODUCT_DEFINITION_SHAPE('',$,#5720);
#5663=PRODUCT_DEFINITION_SHAPE('',$,#5721);
#5664=PRODUCT_DEFINITION_SHAPE('',$,#5722);
#5665=PRODUCT_DEFINITION_SHAPE('',$,#5723);
#5666=PRODUCT_DEFINITION_SHAPE('',$,#5724);
#5667=PRODUCT_DEFINITION_SHAPE('',$,#5725);
#5668=PRODUCT_DEFINITION_SHAPE('',$,#5726);
#5669=PRODUCT_DEFINITION_SHAPE('',$,#5727);
#5670=PRODUCT_DEFINITION_SHAPE('',$,#5728);
#5671=PRODUCT_DEFINITION_SHAPE('',$,#5729);
#5672=PRODUCT_DEFINITION_SHAPE($,$,#93);
#5673=PRODUCT_DEFINITION_SHAPE($,$,#94);
#5674=PRODUCT_DEFINITION_SHAPE('',$,#5730);
#5675=PRODUCT_DEFINITION_SHAPE('',$,#5731);
#5676=PRODUCT_DEFINITION_SHAPE('',$,#5732);
#5677=PRODUCT_DEFINITION_SHAPE($,$,#95);
#5678=PRODUCT_DEFINITION_SHAPE($,$,#96);
#5679=PRODUCT_DEFINITION_SHAPE($,$,#97);
#5680=PRODUCT_DEFINITION_SHAPE($,$,#98);
#5681=PRODUCT_DEFINITION_SHAPE($,$,#99);
#5682=PRODUCT_DEFINITION_SHAPE($,$,#100);
#5683=PRODUCT_DEFINITION_SHAPE($,$,#101);
#5684=PRODUCT_DEFINITION_SHAPE($,$,#102);
#5685=PRODUCT_DEFINITION_SHAPE($,$,#103);
#5686=PRODUCT_DEFINITION_SHAPE($,$,#104);
#5687=PRODUCT_DEFINITION_SHAPE($,$,#105);
#5688=PRODUCT_DEFINITION_SHAPE($,$,#106);
#5689=PRODUCT_DEFINITION_SHAPE($,$,#107);
#5690=PRODUCT_DEFINITION_SHAPE($,$,#108);
#5691=PRODUCT_DEFINITION_SHAPE($,$,#109);
#5692=PRODUCT_DEFINITION_SHAPE($,$,#110);
#5693=PRODUCT_DEFINITION_SHAPE($,$,#111);
#5694=PRODUCT_DEFINITION_SHAPE($,$,#112);
#5695=PRODUCT_DEFINITION_SHAPE($,$,#113);
#5696=PRODUCT_DEFINITION_SHAPE($,$,#114);
#5697=PRODUCT_DEFINITION_SHAPE($,$,#115);
#5698=PRODUCT_DEFINITION_SHAPE($,$,#116);
#5699=PRODUCT_DEFINITION_SHAPE($,$,#117);
#5700=SHAPE_REPRESENTATION('',(#3309,#3649,#3650,#3651,#3652,#3653,#3654,
#3655,#3656,#3657,#3658,#3659,#3660,#3661,#3662,#3663,#3664,#3665,#3666,
#3667,#3668,#3669,#3670,#3671),#5622);
#5701=SHAPE_REPRESENTATION('',(#3310),#5623);
#5702=SHAPE_REPRESENTATION('',(#3396),#5624);
#5703=SHAPE_REPRESENTATION('',(#3416),#5625);
#5704=SHAPE_REPRESENTATION('',(#3436),#5626);
#5705=SHAPE_REPRESENTATION('',(#3456),#5627);
#5706=SHAPE_REPRESENTATION('',(#3476),#5628);
#5707=SHAPE_REPRESENTATION('',(#3506),#5629);
#5708=SHAPE_REPRESENTATION('',(#3536),#5630);
#5709=SHAPE_REPRESENTATION('',(#3558),#5631);
#5710=SHAPE_REPRESENTATION('',(#3571,#3613,#3614),#5632);
#5711=SHAPE_REPRESENTATION('',(#3572),#5633);
#5712=SHAPE_REPRESENTATION('',(#3600),#5634);
#5713=SHAPE_REPRESENTATION('',(#3615),#5635);
#5714=SHAPE_REPRESENTATION('',(#3623),#5636);
#5715=SHAPE_REPRESENTATION('',(#3632),#5637);
#5716=PRODUCT_DEFINITION_CONTEXT('part definition',#5766,'design');
#5717=PRODUCT_DEFINITION('PAT-042',
'PAT-042',#5733,#5716);
#5718=PRODUCT_DEFINITION('Manifold block','Manifold block',#5734,
#5716);
#5719=PRODUCT_DEFINITION('1/4-1/8 in port reducer (3)',
'1/4-1/8 in port reducer (3)',#5735,#5716);
#5720=PRODUCT_DEFINITION('1/4-1/8 in port reducer',
'1/4-1/8 in port reducer',#5736,#5716);
#5721=PRODUCT_DEFINITION('1/4-1/8 in port reducer (1)',
'1/4-1/8 in port reducer (1)',#5737,#5716);
#5722=PRODUCT_DEFINITION('1/4-1/8 in port reducer (2)',
'1/4-1/8 in port reducer (2)',#5738,#5716);
#5723=PRODUCT_DEFINITION('Mounting foot','Mounting foot',#5739,
#5716);
#5724=PRODUCT_DEFINITION('Mounting foot (1)','Mounting foot (1)',
#5740,#5716);
#5725=PRODUCT_DEFINITION('Hex Pipe Nipple - 1-4 Inch Tapered Pipe Thread',
'Hex Pipe Nipple - 1-4 Inch Tapered Pipe Thread',#5741,#5716);
#5726=PRODUCT_DEFINITION('Blanking plug','Blanking plug',#5742,
#5716);
#5727=PRODUCT_DEFINITION('Push-In Tube Fitting - 6 mm Tube, 1-8 Inch Tapered Pipe Thread',
'Push-In Tube Fitting - 6 mm Tube, 1-8 Inch Tapered Pipe Thread',#5743,
#5716);
#5728=PRODUCT_DEFINITION('Body','Body',#5744,#5716);
#5729=PRODUCT_DEFINITION('Release collar','Release collar',#5745,
#5716);
#5730=PRODUCT_DEFINITION('Dowel Pin - 4 x 20 mm',
'Dowel Pin - 4 x 20 mm',#5746,#5716);
#5731=PRODUCT_DEFINITION('Flat Washer - M6','Flat Washer - M6',
#5747,#5716);
#5732=PRODUCT_DEFINITION('Hex Bolt - M6 x 30 mm',
'Hex Bolt - M6 x 30 mm',#5748,#5716);
#5733=PRODUCT_DEFINITION_FORMATION('',$,#5768);
#5734=PRODUCT_DEFINITION_FORMATION('',$,#5769);
#5735=PRODUCT_DEFINITION_FORMATION('',$,#5770);
#5736=PRODUCT_DEFINITION_FORMATION('',$,#5771);
#5737=PRODUCT_DEFINITION_FORMATION('',$,#5772);
#5738=PRODUCT_DEFINITION_FORMATION('',$,#5773);
#5739=PRODUCT_DEFINITION_FORMATION('',$,#5774);
#5740=PRODUCT_DEFINITION_FORMATION('',$,#5775);
#5741=PRODUCT_DEFINITION_FORMATION('',$,#5776);
#5742=PRODUCT_DEFINITION_FORMATION('',$,#5777);
#5743=PRODUCT_DEFINITION_FORMATION('',$,#5778);
#5744=PRODUCT_DEFINITION_FORMATION('',$,#5779);
#5745=PRODUCT_DEFINITION_FORMATION('',$,#5780);
#5746=PRODUCT_DEFINITION_FORMATION('',$,#5781);
#5747=PRODUCT_DEFINITION_FORMATION('',$,#5782);
#5748=PRODUCT_DEFINITION_FORMATION('',$,#5783);
#5749=PRODUCT_RELATED_PRODUCT_CATEGORY(
'PAT-042','PAT-042',(#5768));
#5750=PRODUCT_RELATED_PRODUCT_CATEGORY('Manifold block',
'Manifold block',(#5769));
#5751=PRODUCT_RELATED_PRODUCT_CATEGORY('1/4-1/8 in port reducer (3)',
'1/4-1/8 in port reducer (3)',(#5770));
#5752=PRODUCT_RELATED_PRODUCT_CATEGORY('1/4-1/8 in port reducer',
'1/4-1/8 in port reducer',(#5771));
#5753=PRODUCT_RELATED_PRODUCT_CATEGORY('1/4-1/8 in port reducer (1)',
'1/4-1/8 in port reducer (1)',(#5772));
#5754=PRODUCT_RELATED_PRODUCT_CATEGORY('1/4-1/8 in port reducer (2)',
'1/4-1/8 in port reducer (2)',(#5773));
#5755=PRODUCT_RELATED_PRODUCT_CATEGORY('Mounting foot','Mounting foot',
(#5774));
#5756=PRODUCT_RELATED_PRODUCT_CATEGORY('Mounting foot (1)',
'Mounting foot (1)',(#5775));
#5757=PRODUCT_RELATED_PRODUCT_CATEGORY(
'Hex Pipe Nipple - 1-4 Inch Tapered Pipe Thread',
'Hex Pipe Nipple - 1-4 Inch Tapered Pipe Thread',(#5776));
#5758=PRODUCT_RELATED_PRODUCT_CATEGORY('Blanking plug','Blanking plug',
(#5777));
#5759=PRODUCT_RELATED_PRODUCT_CATEGORY(
'Push-In Tube Fitting - 6 mm Tube, 1-8 Inch Tapered Pipe Thread',
'Push-In Tube Fitting - 6 mm Tube, 1-8 Inch Tapered Pipe Thread',(#5778));
#5760=PRODUCT_RELATED_PRODUCT_CATEGORY('Body','Body',(#5779));
#5761=PRODUCT_RELATED_PRODUCT_CATEGORY('Release collar',
'Release collar',(#5780));
#5762=PRODUCT_RELATED_PRODUCT_CATEGORY('Dowel Pin - 4 x 20 mm',
'Dowel Pin - 4 x 20 mm',(#5781));
#5763=PRODUCT_RELATED_PRODUCT_CATEGORY('Flat Washer - M6',
'Flat Washer - M6',(#5782));
#5764=PRODUCT_RELATED_PRODUCT_CATEGORY('Hex Bolt - M6 x 30 mm',
'Hex Bolt - M6 x 30 mm',(#5783));
#5765=APPLICATION_PROTOCOL_DEFINITION('international standard',
'automotive_design',2009,#5766);
#5766=APPLICATION_CONTEXT(
'Core Data for Automotive Mechanical Design Process');
#5767=PRODUCT_CONTEXT('part definition',#5766,'mechanical');
#5768=PRODUCT('PAT-042',
'PAT-042','PAT-042',(#5767));
#5769=PRODUCT('Manifold block','Manifold block',
'Manifold block',(#5767));
#5770=PRODUCT('1/4-1/8 in port reducer (3)','1/4-1/8 in port reducer (3)',
'1/4-1/8 in port reducer (3)',(#5767));
#5771=PRODUCT('1/4-1/8 in port reducer','1/4-1/8 in port reducer',
'1/4-1/8 in port reducer',(#5767));
#5772=PRODUCT('1/4-1/8 in port reducer (1)','1/4-1/8 in port reducer (1)',
'1/4-1/8 in port reducer (1)',(#5767));
#5773=PRODUCT('1/4-1/8 in port reducer (2)','1/4-1/8 in port reducer (2)',
'1/4-1/8 in port reducer (2)',(#5767));
#5774=PRODUCT('Mounting foot','Mounting foot',
'Mounting foot',(#5767));
#5775=PRODUCT('Mounting foot (1)','Mounting foot (1)',
'Mounting foot (1)',(#5767));
#5776=PRODUCT('Hex Pipe Nipple - 1-4 Inch Tapered Pipe Thread',
'Hex Pipe Nipple - 1-4 Inch Tapered Pipe Thread',
'Hex Pipe Nipple - 1-4 Inch Tapered Pipe Thread',(#5767));
#5777=PRODUCT('Blanking plug','Blanking plug',
'Blanking plug',(#5767));
#5778=PRODUCT('Push-In Tube Fitting - 6 mm Tube, 1-8 Inch Tapered Pipe Thread',
'Push-In Tube Fitting - 6 mm Tube, 1-8 Inch Tapered Pipe Thread',
'Push-In Tube Fitting - 6 mm Tube, 1-8 Inch Tapered Pipe Thread',(#5767));
#5779=PRODUCT('Body','Body','Body',(#5767));
#5780=PRODUCT('Release collar','Release collar',
'Release collar',(#5767));
#5781=PRODUCT('Dowel Pin - 4 x 20 mm','Dowel Pin - 4 x 20 mm',
'Dowel Pin - 4 x 20 mm',(#5767));
#5782=PRODUCT('Flat Washer - M6','Flat Washer - M6',
'Flat Washer - M6',(#5767));
#5783=PRODUCT('Hex Bolt - M6 x 30 mm','Hex Bolt - M6 x 30 mm',
'Hex Bolt - M6 x 30 mm',(#5767));
#5784=PRESENTATION_STYLE_ASSIGNMENT((#5791));
#5785=PRESENTATION_STYLE_ASSIGNMENT((#5792));
#5786=PRESENTATION_STYLE_ASSIGNMENT((#5793));
#5787=PRESENTATION_STYLE_ASSIGNMENT((#5794));
#5788=PRESENTATION_STYLE_ASSIGNMENT((#5795));
#5789=PRESENTATION_STYLE_ASSIGNMENT((#5796));
#5790=PRESENTATION_STYLE_ASSIGNMENT((#5797));
#5791=SURFACE_STYLE_USAGE(.BOTH.,#5798);
#5792=SURFACE_STYLE_USAGE(.BOTH.,#5799);
#5793=SURFACE_STYLE_USAGE(.BOTH.,#5800);
#5794=SURFACE_STYLE_USAGE(.BOTH.,#5801);
#5795=SURFACE_STYLE_USAGE(.BOTH.,#5802);
#5796=SURFACE_STYLE_USAGE(.BOTH.,#5803);
#5797=SURFACE_STYLE_USAGE(.BOTH.,#5804);
#5798=SURFACE_SIDE_STYLE('',(#5805));
#5799=SURFACE_SIDE_STYLE('',(#5806));
#5800=SURFACE_SIDE_STYLE('',(#5807));
#5801=SURFACE_SIDE_STYLE('',(#5808));
#5802=SURFACE_SIDE_STYLE('',(#5809));
#5803=SURFACE_SIDE_STYLE('',(#5810));
#5804=SURFACE_SIDE_STYLE('',(#5811));
#5805=SURFACE_STYLE_FILL_AREA(#5812);
#5806=SURFACE_STYLE_FILL_AREA(#5813);
#5807=SURFACE_STYLE_FILL_AREA(#5814);
#5808=SURFACE_STYLE_FILL_AREA(#5815);
#5809=SURFACE_STYLE_FILL_AREA(#5816);
#5810=SURFACE_STYLE_FILL_AREA(#5817);
#5811=SURFACE_STYLE_FILL_AREA(#5818);
#5812=FILL_AREA_STYLE('Steel - Satin',(#5819));
#5813=FILL_AREA_STYLE('CAD Library Painted - Light blue',(#5820));
#5814=FILL_AREA_STYLE('CAD Library Painted - Engineering blue',(#5821));
#5815=FILL_AREA_STYLE('CAD Library Painted - Deep blue',(#5822));
#5816=FILL_AREA_STYLE('CAD Library Painted - Steel gray',(#5823));
#5817=FILL_AREA_STYLE('CAD Library Painted - Off white',(#5824));
#5818=FILL_AREA_STYLE('CAD Library Painted - Graphite',(#5825));
#5819=FILL_AREA_STYLE_COLOUR('Steel - Satin',#5826);
#5820=FILL_AREA_STYLE_COLOUR('CAD Library Painted - Light blue',#5827);
#5821=FILL_AREA_STYLE_COLOUR('CAD Library Painted - Engineering blue',#5828);
#5822=FILL_AREA_STYLE_COLOUR('CAD Library Painted - Deep blue',#5829);
#5823=FILL_AREA_STYLE_COLOUR('CAD Library Painted - Steel gray',#5830);
#5824=FILL_AREA_STYLE_COLOUR('CAD Library Painted - Off white',#5831);
#5825=FILL_AREA_STYLE_COLOUR('CAD Library Painted - Graphite',#5832);
#5826=COLOUR_RGB('Steel - Satin',0.627450980392157,0.627450980392157,0.627450980392157);
#5827=COLOUR_RGB('CAD Library Painted - Light blue',0.286274509803922,0.552941176470588,
0.780392156862745);
#5828=COLOUR_RGB('CAD Library Painted - Engineering blue',0.12156862745098,
0.356862745098039,0.6);
#5829=COLOUR_RGB('CAD Library Painted - Deep blue',0.0784313725490196,0.203921568627451,
0.349019607843137);
#5830=COLOUR_RGB('CAD Library Painted - Steel gray',0.592156862745098,0.631372549019608,
0.67843137254902);
#5831=COLOUR_RGB('CAD Library Painted - Off white',0.909803921568627,0.901960784313726,
0.858823529411765);
#5832=COLOUR_RGB('CAD Library Painted - Graphite',0.0980392156862745,0.109803921568627,
0.125490196078431);
#5833=COLOUR_RGB('Dark Blue',0.08,0.2,0.34);
#5834=FILL_AREA_STYLE_COLOUR('',#5833);
#5835=FILL_AREA_STYLE('',(#5834));
#5836=SURFACE_STYLE_FILL_AREA(#5835);
#5837=SURFACE_SIDE_STYLE('',(#5836));
#5838=SURFACE_STYLE_USAGE(.BOTH.,#5837);
#5839=PRESENTATION_STYLE_ASSIGNMENT((#5838));
#5840=COLOUR_RGB('Light Blue',0.38,0.62,0.78);
#5841=FILL_AREA_STYLE_COLOUR('',#5840);
#5842=FILL_AREA_STYLE('',(#5841));
#5843=SURFACE_STYLE_FILL_AREA(#5842);
#5844=SURFACE_SIDE_STYLE('',(#5843));
#5845=SURFACE_STYLE_USAGE(.BOTH.,#5844);
#5846=PRESENTATION_STYLE_ASSIGNMENT((#5845));
#5847=COLOUR_RGB('Sky Blue',0.24,0.69,0.87);
#5848=FILL_AREA_STYLE_COLOUR('',#5847);
#5849=FILL_AREA_STYLE('',(#5848));
#5850=SURFACE_STYLE_FILL_AREA(#5849);
#5851=SURFACE_SIDE_STYLE('',(#5850));
#5852=SURFACE_STYLE_USAGE(.BOTH.,#5851);
#5853=PRESENTATION_STYLE_ASSIGNMENT((#5852));
#5854=COLOUR_RGB('Grey',0.48,0.52,0.57);
#5855=FILL_AREA_STYLE_COLOUR('',#5854);
#5856=FILL_AREA_STYLE('',(#5855));
#5857=SURFACE_STYLE_FILL_AREA(#5856);
#5858=SURFACE_SIDE_STYLE('',(#5857));
#5859=SURFACE_STYLE_USAGE(.BOTH.,#5858);
#5860=PRESENTATION_STYLE_ASSIGNMENT((#5859));
#5861=COLOUR_RGB('Black',0.12,0.14,0.17);
#5862=FILL_AREA_STYLE_COLOUR('',#5861);
#5863=FILL_AREA_STYLE('',(#5862));
#5864=SURFACE_STYLE_FILL_AREA(#5863);
#5865=SURFACE_SIDE_STYLE('',(#5864));
#5866=SURFACE_STYLE_USAGE(.BOTH.,#5865);
#5867=PRESENTATION_STYLE_ASSIGNMENT((#5866));
#5868=COLOUR_RGB('Off White',0.89,0.88,0.83);
#5869=FILL_AREA_STYLE_COLOUR('',#5868);
#5870=FILL_AREA_STYLE('',(#5869));
#5871=SURFACE_STYLE_FILL_AREA(#5870);
#5872=SURFACE_SIDE_STYLE('',(#5871));
#5873=SURFACE_STYLE_USAGE(.BOTH.,#5872);
#5874=PRESENTATION_STYLE_ASSIGNMENT((#5873));
ENDSEC;
END-ISO-10303-21;
